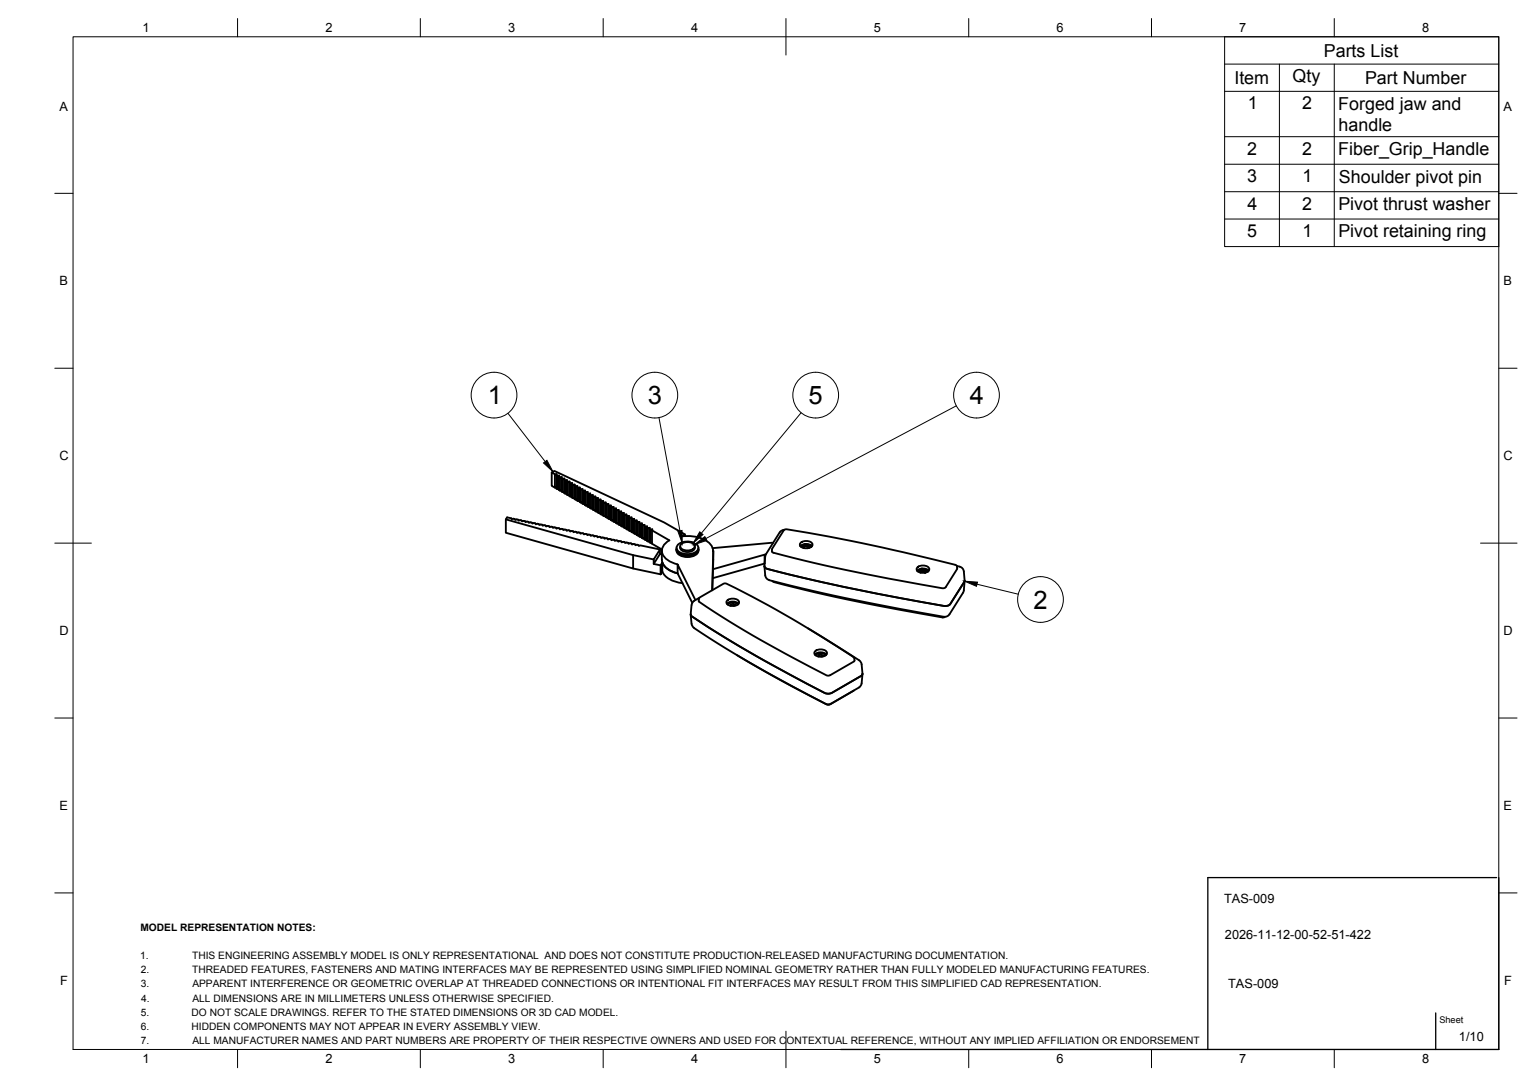
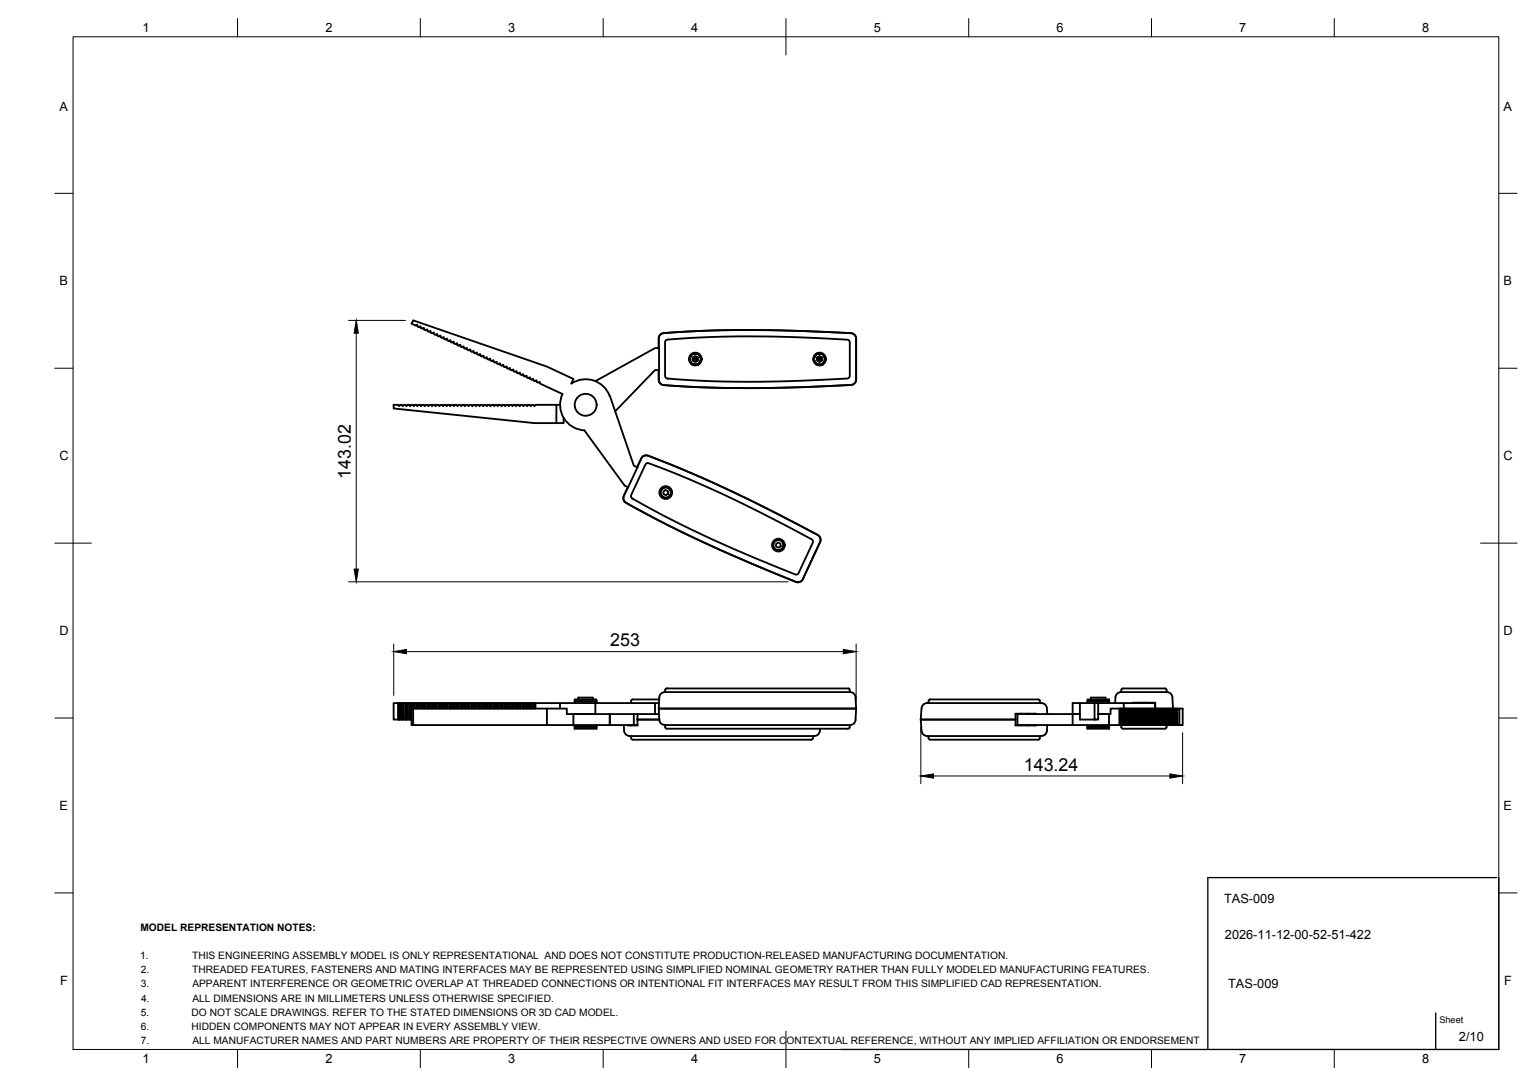
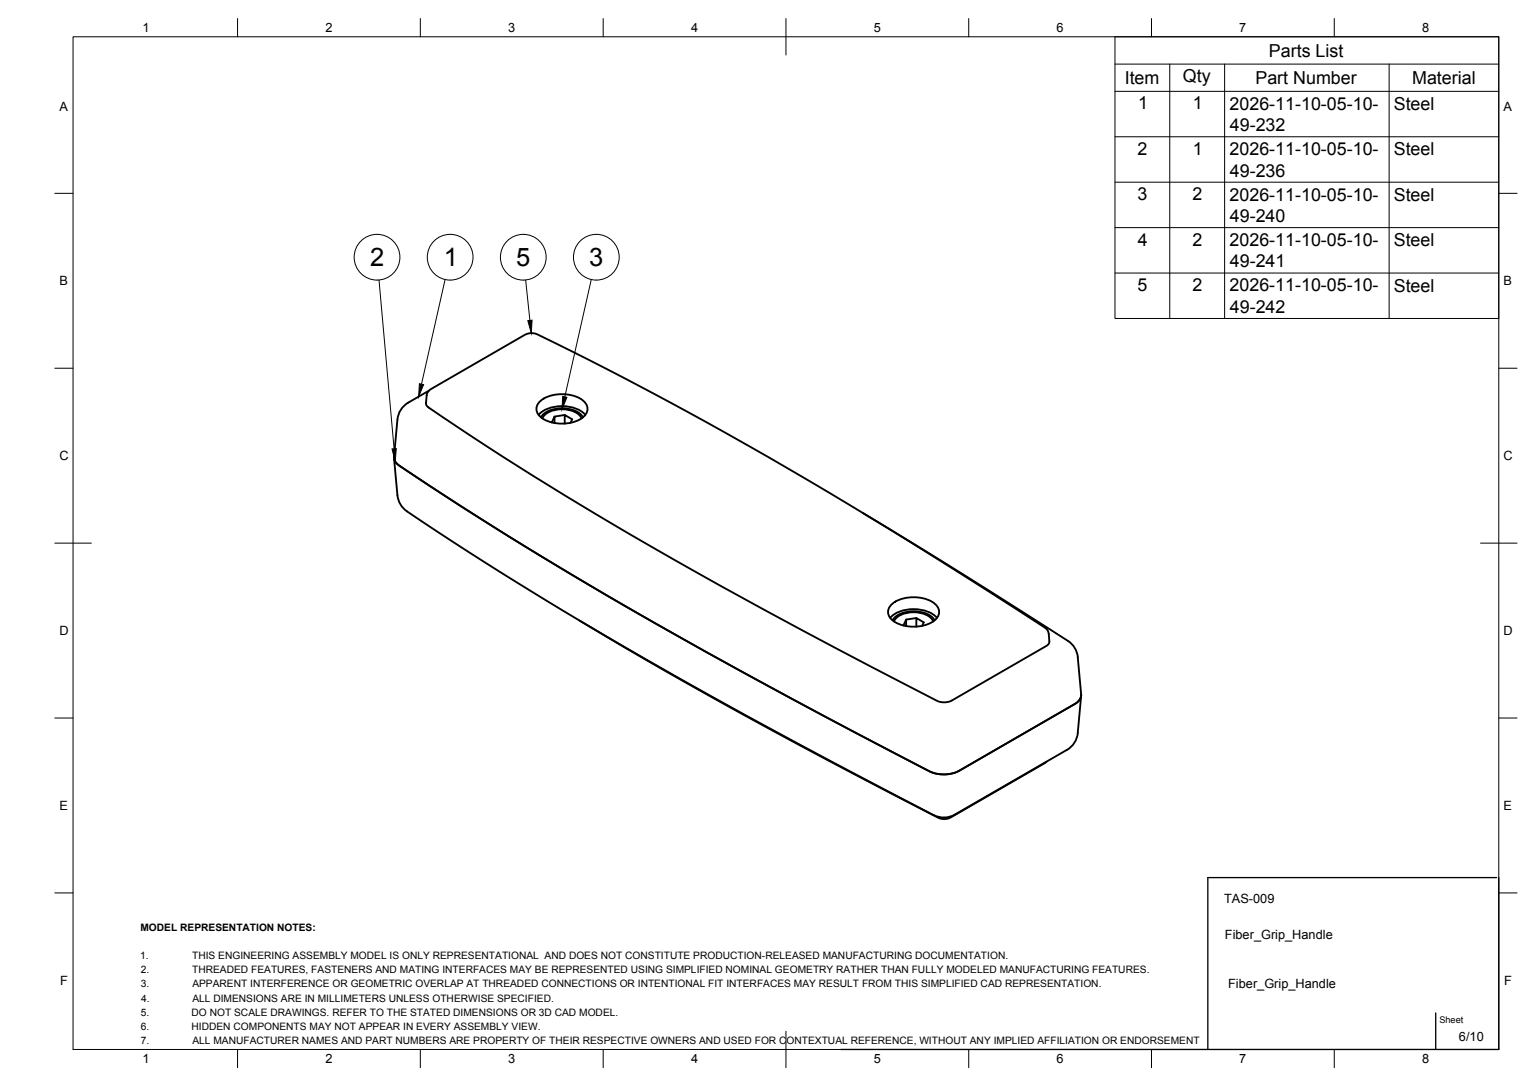
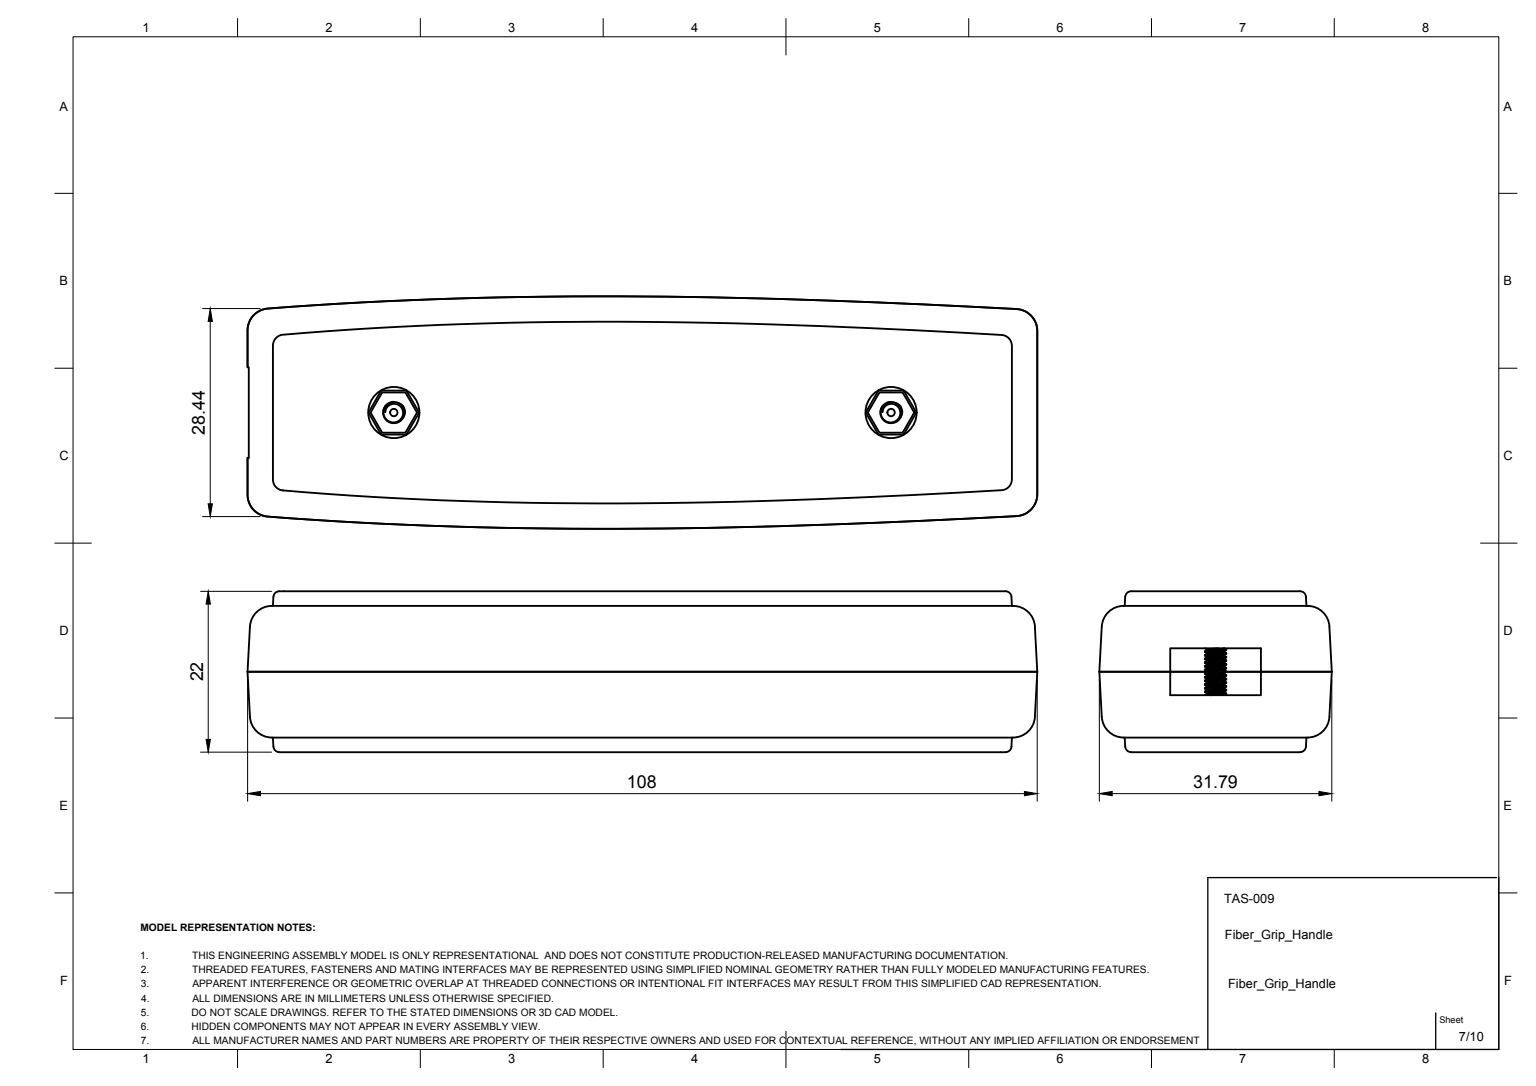
ISO-10303-21;
HEADER;
/* Generated by software containing ST-Developer
 * from STEP Tools, Inc. (www.steptools.com) 
 */

FILE_DESCRIPTION(
/* description */ (''),
/* implementation_level */ '2;1');

FILE_NAME(
/* name */ 'TAS-009.step',
/* time_stamp */ '2026-11-12T00:53:40-08:00',
/* author */ (''),
/* organization */ (''),
/* preprocessor_version */ 'ST-DEVELOPER v20.2',
/* originating_system */ 'Autodesk Translation Framework v15.17.0.0',
/* authorisation */ '');

FILE_SCHEMA (('AUTOMOTIVE_DESIGN { 1 0 10303 214 3 1 1 }'));
ENDSEC;

DATA;
#10=MECHANICAL_DESIGN_GEOMETRIC_PRESENTATION_REPRESENTATION('',(#572,#573,
#574,#575,#576,#577,#578,#579,#580),#22129);
#11=ITEM_DEFINED_TRANSFORMATION($,$,#9088,#9475);
#12=ITEM_DEFINED_TRANSFORMATION($,$,#9198,#9476);
#13=ITEM_DEFINED_TRANSFORMATION($,$,#9314,#9477);
#14=ITEM_DEFINED_TRANSFORMATION($,$,#9396,#9478);
#15=ITEM_DEFINED_TRANSFORMATION($,$,#9422,#9479);
#16=ITEM_DEFINED_TRANSFORMATION($,$,#9314,#9480);
#17=ITEM_DEFINED_TRANSFORMATION($,$,#9396,#9481);
#18=ITEM_DEFINED_TRANSFORMATION($,$,#9422,#9482);
#19=ITEM_DEFINED_TRANSFORMATION($,$,#8913,#9492);
#20=ITEM_DEFINED_TRANSFORMATION($,$,#9087,#9493);
#21=ITEM_DEFINED_TRANSFORMATION($,$,#8913,#9494);
#22=ITEM_DEFINED_TRANSFORMATION($,$,#9058,#9495);
#23=ITEM_DEFINED_TRANSFORMATION($,$,#9483,#9496);
#24=ITEM_DEFINED_TRANSFORMATION($,$,#9076,#9497);
#25=ITEM_DEFINED_TRANSFORMATION($,$,#9087,#9498);
#26=ITEM_DEFINED_TRANSFORMATION($,$,#9483,#9499);
#27=(
REPRESENTATION_RELATIONSHIP($,$,#22177,#22176)
REPRESENTATION_RELATIONSHIP_WITH_TRANSFORMATION(#11)
SHAPE_REPRESENTATION_RELATIONSHIP()
);
#28=(
REPRESENTATION_RELATIONSHIP($,$,#22178,#22176)
REPRESENTATION_RELATIONSHIP_WITH_TRANSFORMATION(#12)
SHAPE_REPRESENTATION_RELATIONSHIP()
);
#29=(
REPRESENTATION_RELATIONSHIP($,$,#22179,#22176)
REPRESENTATION_RELATIONSHIP_WITH_TRANSFORMATION(#13)
SHAPE_REPRESENTATION_RELATIONSHIP()
);
#30=(
REPRESENTATION_RELATIONSHIP($,$,#22180,#22176)
REPRESENTATION_RELATIONSHIP_WITH_TRANSFORMATION(#14)
SHAPE_REPRESENTATION_RELATIONSHIP()
);
#31=(
REPRESENTATION_RELATIONSHIP($,$,#22181,#22176)
REPRESENTATION_RELATIONSHIP_WITH_TRANSFORMATION(#15)
SHAPE_REPRESENTATION_RELATIONSHIP()
);
#32=(
REPRESENTATION_RELATIONSHIP($,$,#22179,#22176)
REPRESENTATION_RELATIONSHIP_WITH_TRANSFORMATION(#16)
SHAPE_REPRESENTATION_RELATIONSHIP()
);
#33=(
REPRESENTATION_RELATIONSHIP($,$,#22180,#22176)
REPRESENTATION_RELATIONSHIP_WITH_TRANSFORMATION(#17)
SHAPE_REPRESENTATION_RELATIONSHIP()
);
#34=(
REPRESENTATION_RELATIONSHIP($,$,#22181,#22176)
REPRESENTATION_RELATIONSHIP_WITH_TRANSFORMATION(#18)
SHAPE_REPRESENTATION_RELATIONSHIP()
);
#35=(
REPRESENTATION_RELATIONSHIP($,$,#22173,#22172)
REPRESENTATION_RELATIONSHIP_WITH_TRANSFORMATION(#19)
SHAPE_REPRESENTATION_RELATIONSHIP()
);
#36=(
REPRESENTATION_RELATIONSHIP($,$,#22176,#22172)
REPRESENTATION_RELATIONSHIP_WITH_TRANSFORMATION(#20)
SHAPE_REPRESENTATION_RELATIONSHIP()
);
#37=(
REPRESENTATION_RELATIONSHIP($,$,#22173,#22172)
REPRESENTATION_RELATIONSHIP_WITH_TRANSFORMATION(#21)
SHAPE_REPRESENTATION_RELATIONSHIP()
);
#38=(
REPRESENTATION_RELATIONSHIP($,$,#22174,#22172)
REPRESENTATION_RELATIONSHIP_WITH_TRANSFORMATION(#22)
SHAPE_REPRESENTATION_RELATIONSHIP()
);
#39=(
REPRESENTATION_RELATIONSHIP($,$,#22182,#22172)
REPRESENTATION_RELATIONSHIP_WITH_TRANSFORMATION(#23)
SHAPE_REPRESENTATION_RELATIONSHIP()
);
#40=(
REPRESENTATION_RELATIONSHIP($,$,#22175,#22172)
REPRESENTATION_RELATIONSHIP_WITH_TRANSFORMATION(#24)
SHAPE_REPRESENTATION_RELATIONSHIP()
);
#41=(
REPRESENTATION_RELATIONSHIP($,$,#22176,#22172)
REPRESENTATION_RELATIONSHIP_WITH_TRANSFORMATION(#25)
SHAPE_REPRESENTATION_RELATIONSHIP()
);
#42=(
REPRESENTATION_RELATIONSHIP($,$,#22182,#22172)
REPRESENTATION_RELATIONSHIP_WITH_TRANSFORMATION(#26)
SHAPE_REPRESENTATION_RELATIONSHIP()
);
#43=CONTEXT_DEPENDENT_SHAPE_REPRESENTATION(#27,#22155);
#44=CONTEXT_DEPENDENT_SHAPE_REPRESENTATION(#28,#22156);
#45=CONTEXT_DEPENDENT_SHAPE_REPRESENTATION(#29,#22157);
#46=CONTEXT_DEPENDENT_SHAPE_REPRESENTATION(#30,#22158);
#47=CONTEXT_DEPENDENT_SHAPE_REPRESENTATION(#31,#22159);
#48=CONTEXT_DEPENDENT_SHAPE_REPRESENTATION(#32,#22160);
#49=CONTEXT_DEPENDENT_SHAPE_REPRESENTATION(#33,#22161);
#50=CONTEXT_DEPENDENT_SHAPE_REPRESENTATION(#34,#22162);
#51=CONTEXT_DEPENDENT_SHAPE_REPRESENTATION(#35,#22164);
#52=CONTEXT_DEPENDENT_SHAPE_REPRESENTATION(#36,#22165);
#53=CONTEXT_DEPENDENT_SHAPE_REPRESENTATION(#37,#22166);
#54=CONTEXT_DEPENDENT_SHAPE_REPRESENTATION(#38,#22167);
#55=CONTEXT_DEPENDENT_SHAPE_REPRESENTATION(#39,#22168);
#56=CONTEXT_DEPENDENT_SHAPE_REPRESENTATION(#40,#22169);
#57=CONTEXT_DEPENDENT_SHAPE_REPRESENTATION(#41,#22170);
#58=CONTEXT_DEPENDENT_SHAPE_REPRESENTATION(#42,#22171);
#59=NEXT_ASSEMBLY_USAGE_OCCURRENCE('Upper structural shell:1',
'Upper structural shell:1','Upper structural shell:1',#22188,#22189,
'Upper structural shell:1');
#60=NEXT_ASSEMBLY_USAGE_OCCURRENCE('Lower structural shell:1',
'Lower structural shell:1','Lower structural shell:1',#22188,#22190,
'Lower structural shell:1');
#61=NEXT_ASSEMBLY_USAGE_OCCURRENCE('Socket head cap screw M3x16:1',
'Socket head cap screw M3x16:1','Socket head cap screw M3x16:1',#22188,
#22191,'Socket head cap screw M3x16:1');
#62=NEXT_ASSEMBLY_USAGE_OCCURRENCE('Hex nut M3:1','Hex nut M3:1',
'Hex nut M3:1',#22188,#22192,'Hex nut M3:1');
#63=NEXT_ASSEMBLY_USAGE_OCCURRENCE('Soft grip layer:1',
'Soft grip layer:1','Soft grip layer:1',#22188,#22193,
'Soft grip layer:1');
#64=NEXT_ASSEMBLY_USAGE_OCCURRENCE('Socket head cap screw M3x16:2',
'Socket head cap screw M3x16:2','Socket head cap screw M3x16:2',#22188,
#22191,'Socket head cap screw M3x16:2');
#65=NEXT_ASSEMBLY_USAGE_OCCURRENCE('Hex nut M3:2','Hex nut M3:2',
'Hex nut M3:2',#22188,#22192,'Hex nut M3:2');
#66=NEXT_ASSEMBLY_USAGE_OCCURRENCE('Soft grip layer:2',
'Soft grip layer:2','Soft grip layer:2',#22188,#22193,
'Soft grip layer:2');
#67=NEXT_ASSEMBLY_USAGE_OCCURRENCE('Forged jaw and handle:1',
'Forged jaw and handle:1','Forged jaw and handle:1',#22184,#22185,
'Forged jaw and handle:1');
#68=NEXT_ASSEMBLY_USAGE_OCCURRENCE('Fiber_Grip_Handle:1',
'Fiber_Grip_Handle:1','Fiber_Grip_Handle:1',#22184,#22188,
'Fiber_Grip_Handle:1');
#69=NEXT_ASSEMBLY_USAGE_OCCURRENCE('Forged jaw and handle:2',
'Forged jaw and handle:2','Forged jaw and handle:2',#22184,#22185,
'Forged jaw and handle:2');
#70=NEXT_ASSEMBLY_USAGE_OCCURRENCE('Shoulder pivot pin:1',
'Shoulder pivot pin:1','Shoulder pivot pin:1',#22184,#22186,
'Shoulder pivot pin:1');
#71=NEXT_ASSEMBLY_USAGE_OCCURRENCE('Pivot thrust washer:1',
'Pivot thrust washer:1','Pivot thrust washer:1',#22184,#22194,
'Pivot thrust washer:1');
#72=NEXT_ASSEMBLY_USAGE_OCCURRENCE('Pivot retaining ring:1',
'Pivot retaining ring:1','Pivot retaining ring:1',#22184,#22187,
'Pivot retaining ring:1');
#73=NEXT_ASSEMBLY_USAGE_OCCURRENCE('Fiber_Grip_Handle:2',
'Fiber_Grip_Handle:2','Fiber_Grip_Handle:2',#22184,#22188,
'Fiber_Grip_Handle:2');
#74=NEXT_ASSEMBLY_USAGE_OCCURRENCE('Pivot thrust washer:2',
'Pivot thrust washer:2','Pivot thrust washer:2',#22184,#22194,
'Pivot thrust washer:2');
#75=CONICAL_SURFACE('',#9377,0.1,0.785398163397448);
#76=SPHERICAL_SURFACE('',#9161,0.1);
#77=SPHERICAL_SURFACE('',#9164,0.0999999999999998);
#78=SPHERICAL_SURFACE('',#9168,0.0999999999999993);
#79=SPHERICAL_SURFACE('',#9172,0.1);
#80=SPHERICAL_SURFACE('',#9177,0.3);
#81=SPHERICAL_SURFACE('',#9181,0.3);
#82=SPHERICAL_SURFACE('',#9185,0.299999999999999);
#83=SPHERICAL_SURFACE('',#9190,0.3);
#84=SPHERICAL_SURFACE('',#9277,0.1);
#85=SPHERICAL_SURFACE('',#9280,0.0999999999999998);
#86=SPHERICAL_SURFACE('',#9284,0.0999999999999993);
#87=SPHERICAL_SURFACE('',#9288,0.1);
#88=SPHERICAL_SURFACE('',#9293,0.3);
#89=SPHERICAL_SURFACE('',#9297,0.3);
#90=SPHERICAL_SURFACE('',#9301,0.299999999999999);
#91=SPHERICAL_SURFACE('',#9306,0.3);
#92=B_SPLINE_SURFACE_WITH_KNOTS('',3,3,((#12365,#12366,#12367,#12368),(#12369,
#12370,#12371,#12372),(#12373,#12374,#12375,#12376),(#12377,#12378,#12379,
#12380),(#12381,#12382,#12383,#12384)),.UNSPECIFIED.,.F.,.F.,.F.,(4,1,4),
(4,4),(0.,0.571428571428571,1.),(1.0454440030657,3.44967454744645),
 .UNSPECIFIED.);
#93=B_SPLINE_SURFACE_WITH_KNOTS('',3,3,((#12457,#12458,#12459,#12460),(#12461,
#12462,#12463,#12464),(#12465,#12466,#12467,#12468),(#12469,#12470,#12471,
#12472),(#12473,#12474,#12475,#12476)),.UNSPECIFIED.,.F.,.F.,.F.,(4,1,4),
(4,4),(0.,0.571428571428571,1.),(7.24519303641511,9.95046872158573),
 .UNSPECIFIED.);
#94=B_SPLINE_SURFACE_WITH_KNOTS('',3,3,((#13338,#13339,#13340,#13341),(#13342,
#13343,#13344,#13345),(#13346,#13347,#13348,#13349),(#13350,#13351,#13352,
#13353)),.UNSPECIFIED.,.F.,.F.,.F.,(4,4),(4,4),(0.0705535719740953,0.323522444336189),
(0.0117434863834119,0.684857763552191),.UNSPECIFIED.);
#95=B_SPLINE_SURFACE_WITH_KNOTS('',3,3,((#13358,#13359,#13360,#13361),(#13362,
#13363,#13364,#13365),(#13366,#13367,#13368,#13369),(#13370,#13371,#13372,
#13373)),.UNSPECIFIED.,.F.,.F.,.F.,(4,4),(4,4),(0.0262419052680539,0.0545428296147404),
(0.0121538053864343,0.684980602226481),.UNSPECIFIED.);
#96=B_SPLINE_SURFACE_WITH_KNOTS('',3,3,((#13383,#13384,#13385,#13386),(#13387,
#13388,#13389,#13390),(#13391,#13392,#13393,#13394),(#13395,#13396,#13397,
#13398),(#13399,#13400,#13401,#13402)),.UNSPECIFIED.,.F.,.F.,.F.,(4,1,4),
(4,4),(0.,0.571428571428571,1.),(0.752061768057538,3.45733745322815),
 .UNSPECIFIED.);
#97=B_SPLINE_SURFACE_WITH_KNOTS('',3,3,((#13403,#13404,#13405,#13406),(#13407,
#13408,#13409,#13410),(#13411,#13412,#13413,#13414),(#13415,#13416,#13417,
#13418),(#13419,#13420,#13421,#13422)),.UNSPECIFIED.,.F.,.F.,.F.,(4,1,4),
(4,4),(0.,0.571428571428571,1.),(0.283259008618247,0.557056952888827),
 .UNSPECIFIED.);
#98=B_SPLINE_SURFACE_WITH_KNOTS('',3,3,((#13436,#13437,#13438,#13439),(#13440,
#13441,#13442,#13443),(#13444,#13445,#13446,#13447),(#13448,#13449,#13450,
#13451)),.UNSPECIFIED.,.F.,.F.,.F.,(4,4),(4,4),(0.67647755566375,0.929446428026011),
(0.0117434863436937,0.684857763580381),.UNSPECIFIED.);
#99=B_SPLINE_SURFACE_WITH_KNOTS('',3,3,((#13452,#13453,#13454,#13455),(#13456,
#13457,#13458,#13459),(#13460,#13461,#13462,#13463),(#13464,#13465,#13466,
#13467)),.UNSPECIFIED.,.F.,.F.,.F.,(4,4),(4,4),(0.945457170385156,0.973758094731946),
(0.0121538053598088,0.684980602226481),.UNSPECIFIED.);
#100=B_SPLINE_SURFACE_WITH_KNOTS('',3,3,((#13551,#13552,#13553,#13554),
(#13555,#13556,#13557,#13558),(#13559,#13560,#13561,#13562),(#13563,#13564,
#13565,#13566)),.UNSPECIFIED.,.F.,.F.,.F.,(4,4),(4,4),(0.341142793678372,
0.658675488550287),(0.0116221239297273,0.684255166525269),.UNSPECIFIED.);
#101=B_SPLINE_SURFACE_WITH_KNOTS('',3,3,((#13571,#13572,#13573,#13574),
(#13575,#13576,#13577,#13578),(#13579,#13580,#13581,#13582),(#13583,#13584,
#13585,#13586),(#13587,#13588,#13589,#13590)),.UNSPECIFIED.,.F.,.F.,.F.,
(4,1,4),(4,4),(0.,0.571428571428571,1.),(3.65450559744172,7.0548588409572),
 .UNSPECIFIED.);
#102=B_SPLINE_SURFACE_WITH_KNOTS('',3,3,((#13600,#13601,#13602,#13603),
(#13604,#13605,#13606,#13607),(#13608,#13609,#13610,#13611),(#13612,#13613,
#13614,#13615),(#13616,#13617,#13618,#13619)),.UNSPECIFIED.,.F.,.F.,.F.,
(4,1,4),(4,4),(0.,0.571428571428571,1.),(3.64767164868607,7.04802489220155),
 .UNSPECIFIED.);
#103=B_SPLINE_SURFACE_WITH_KNOTS('',3,3,((#13624,#13625,#13626,#13627),
(#13628,#13629,#13630,#13631),(#13632,#13633,#13634,#13635),(#13636,#13637,
#13638,#13639)),.UNSPECIFIED.,.F.,.F.,.F.,(4,4),(4,4),(0.341324511449716,
0.658857206321627),(0.0116221214776208,0.684255166525269),.UNSPECIFIED.);
#104=B_SPLINE_SURFACE_WITH_KNOTS('',3,3,((#13684,#13685,#13686,#13687),
(#13688,#13689,#13690,#13691),(#13692,#13693,#13694,#13695),(#13696,#13697,
#13698,#13699)),.UNSPECIFIED.,.F.,.F.,.F.,(4,4),(4,4),(0.676316266718331,
0.901708040522105),(0.0117102006467275,0.68495201331719),.UNSPECIFIED.);
#105=B_SPLINE_SURFACE_WITH_KNOTS('',3,3,((#13704,#13705,#13706,#13707),
(#13708,#13709,#13710,#13711),(#13712,#13713,#13714,#13715),(#13716,#13717,
#13718,#13719),(#13720,#13721,#13722,#13723)),.UNSPECIFIED.,.F.,.F.,.F.,
(4,1,4),(4,4),(0.,0.571428571428571,1.),(7.25285594219682,9.65708648657758),
 .UNSPECIFIED.);
#106=B_SPLINE_SURFACE_WITH_KNOTS('',3,3,((#13733,#13734,#13735,#13736),
(#13737,#13738,#13739,#13740),(#13741,#13742,#13743,#13744),(#13745,#13746,
#13747,#13748)),.UNSPECIFIED.,.F.,.F.,.F.,(4,4),(4,4),(0.0982919594778951,
0.323683733281714),(0.0117102006467272,0.68495201331719),.UNSPECIFIED.);
#107=B_SPLINE_SURFACE_WITH_KNOTS('',3,3,((#13823,#13824,#13825,#13826),
(#13827,#13828,#13829,#13830),(#13831,#13832,#13833,#13834),(#13835,#13836,
#13837,#13838)),.UNSPECIFIED.,.F.,.F.,.F.,(4,4),(4,4),(0.917922863855343,
0.974411608827007),(0.0122403473423911,0.685344304754238),.UNSPECIFIED.);
#108=B_SPLINE_SURFACE_WITH_KNOTS('',3,3,((#13848,#13849,#13850,#13851),
(#13852,#13853,#13854,#13855),(#13856,#13857,#13858,#13859),(#13860,#13861,
#13862,#13863),(#13864,#13865,#13866,#13867)),.UNSPECIFIED.,.F.,.F.,.F.,
(4,1,4),(4,4),(0.,0.571428571428571,1.),(9.85085636625011,10.4271318523291),
 .UNSPECIFIED.);
#109=B_SPLINE_SURFACE_WITH_KNOTS('',3,3,((#13881,#13882,#13883,#13884),
(#13885,#13886,#13887,#13888),(#13889,#13890,#13891,#13892),(#13893,#13894,
#13895,#13896)),.UNSPECIFIED.,.F.,.F.,.F.,(4,4),(4,4),(0.025588391172993,
0.0820771361446569),(0.0122403473423911,0.685344304754238),
 .UNSPECIFIED.);
#110=B_SPLINE_SURFACE_WITH_KNOTS('',3,3,((#13906,#13907,#13908,#13909),
(#13910,#13911,#13912,#13913),(#13914,#13915,#13916,#13917),(#13918,#13919,
#13920,#13921),(#13922,#13923,#13924,#13925)),.UNSPECIFIED.,.F.,.F.,.F.,
(4,1,4),(4,4),(0.,0.571428571428571,1.),(0.27539863731415,0.851674123393175),
 .UNSPECIFIED.);
#111=B_SPLINE_SURFACE_WITH_KNOTS('',3,3,((#13939,#13940,#13941,#13942),
(#13943,#13944,#13945,#13946),(#13947,#13948,#13949,#13950),(#13951,#13952,
#13953,#13954),(#13955,#13956,#13957,#13958)),.UNSPECIFIED.,.F.,.F.,.F.,
(4,1,4),(4,4),(0.,0.571428571428571,1.),(0.00944995813270487,0.618489359031386),
 .UNSPECIFIED.);
#112=B_SPLINE_SURFACE_WITH_KNOTS('',3,3,((#13965,#13966,#13967,#13968),
(#13969,#13970,#13971,#13972),(#13973,#13974,#13975,#13976),(#13977,#13978,
#13979,#13980),(#13981,#13982,#13983,#13984)),.UNSPECIFIED.,.F.,.F.,.F.,
(4,1,4),(4,4),(0.,0.571428571428571,1.),(0.00908570715245136,0.618164468641375),
 .UNSPECIFIED.);
#113=B_SPLINE_SURFACE_WITH_KNOTS('',3,3,((#13989,#13990,#13991,#13992),
(#13993,#13994,#13995,#13996),(#13997,#13998,#13999,#14000),(#14001,#14002,
#14003,#14004),(#14005,#14006,#14007,#14008)),.UNSPECIFIED.,.F.,.F.,.F.,
(4,1,4),(4,4),(0.,0.571428571428571,1.),(0.0091183540525243,0.618164468641375),
 .UNSPECIFIED.);
#114=B_SPLINE_SURFACE_WITH_KNOTS('',3,3,((#14013,#14014,#14015,#14016),
(#14017,#14018,#14019,#14020),(#14021,#14022,#14023,#14024),(#14025,#14026,
#14027,#14028),(#14029,#14030,#14031,#14032)),.UNSPECIFIED.,.F.,.F.,.F.,
(4,1,4),(4,4),(0.,0.571428571428571,1.),(10.1454735367545,10.419271481025),
 .UNSPECIFIED.);
#115=B_SPLINE_SURFACE_WITH_KNOTS('',3,3,((#14033,#14034,#14035,#14036),
(#14037,#14038,#14039,#14040),(#14041,#14042,#14043,#14044),(#14045,#14046,
#14047,#14048),(#14049,#14050,#14051,#14052)),.UNSPECIFIED.,.F.,.F.,.F.,
(4,1,4),(4,4),(0.,0.571428571428571,1.),(0.0094045468285345,0.618489359031386),
 .UNSPECIFIED.);
#116=B_SPLINE_SURFACE_WITH_KNOTS('',3,3,((#14078,#14079,#14080,#14081),
(#14082,#14083,#14084,#14085),(#14086,#14087,#14088,#14089),(#14090,#14091,
#14092,#14093),(#14094,#14095,#14096,#14097)),.UNSPECIFIED.,.F.,.F.,.F.,
(4,1,4),(4,4),(0.,0.571428571428571,1.),(-0.00535061636073277,0.618489359031386),
 .UNSPECIFIED.);
#117=B_SPLINE_SURFACE_WITH_KNOTS('',3,3,((#14116,#14117,#14118,#14119,#14120),
(#14121,#14122,#14123,#14124,#14125),(#14126,#14127,#14128,#14129,#14130),
(#14131,#14132,#14133,#14134,#14135),(#14136,#14137,#14138,#14139,#14140)),
 .UNSPECIFIED.,.F.,.F.,.F.,(4,1,4),(4,1,4),(0.,0.571428571428571,1.),(0.283259008618247,
4.63063308449434,10.4271318523291),.UNSPECIFIED.);
#118=B_SPLINE_SURFACE_WITH_KNOTS('',3,3,((#14151,#14152,#14153,#14154),
(#14155,#14156,#14157,#14158),(#14159,#14160,#14161,#14162),(#14163,#14164,
#14165,#14166),(#14167,#14168,#14169,#14170)),.UNSPECIFIED.,.F.,.F.,.F.,
(4,1,4),(4,4),(0.,0.571428571428571,1.),(-0.00578978989683084,0.618164468641375),
 .UNSPECIFIED.);
#119=B_SPLINE_SURFACE_WITH_KNOTS('',3,3,((#14179,#14180,#14181,#14182),
(#14183,#14184,#14185,#14186),(#14187,#14188,#14189,#14190),(#14191,#14192,
#14193,#14194),(#14195,#14196,#14197,#14198)),.UNSPECIFIED.,.F.,.F.,.F.,
(4,1,4),(4,4),(0.,0.571428571428571,1.),(-0.00569189159989896,0.618164468641375),
 .UNSPECIFIED.);
#120=B_SPLINE_SURFACE_WITH_KNOTS('',3,3,((#14207,#14208,#14209,#14210,#14211),
(#14212,#14213,#14214,#14215,#14216),(#14217,#14218,#14219,#14220,#14221),
(#14222,#14223,#14224,#14225,#14226),(#14227,#14228,#14229,#14230,#14231)),
 .UNSPECIFIED.,.F.,.F.,.F.,(4,1,4),(4,1,4),(0.,0.571428571428571,1.),(0.27539863731415,
4.62277271319024,10.419271481025),.UNSPECIFIED.);
#121=B_SPLINE_SURFACE_WITH_KNOTS('',3,3,((#14242,#14243,#14244,#14245),
(#14246,#14247,#14248,#14249),(#14250,#14251,#14252,#14253),(#14254,#14255,
#14256,#14257),(#14258,#14259,#14260,#14261)),.UNSPECIFIED.,.F.,.F.,.F.,
(4,1,4),(4,4),(0.,0.571428571428571,1.),(-0.0054868135546625,0.618489359031386),
 .UNSPECIFIED.);
#122=B_SPLINE_SURFACE_WITH_KNOTS('',3,3,((#14270,#14271,#14272,#14273),
(#14274,#14275,#14276,#14277),(#14278,#14279,#14280,#14281),(#14282,#14283,
#14284,#14285)),.UNSPECIFIED.,.F.,.F.,.F.,(4,4),(4,4),(0.026239262514127,
0.974414173651419),(0.,0.685344304754238),.UNSPECIFIED.);
#123=B_SPLINE_SURFACE_WITH_KNOTS('',3,3,((#14288,#14289,#14290,#14291),
(#14292,#14293,#14294,#14295),(#14296,#14297,#14298,#14299),(#14300,#14301,
#14302,#14303)),.UNSPECIFIED.,.F.,.F.,.F.,(4,4),(4,4),(0.0255858263485814,
0.973760737485873),(0.,0.685344304754238),.UNSPECIFIED.);
#124=B_SPLINE_SURFACE_WITH_KNOTS('',3,3,((#14410,#14411,#14412,#14413),
(#14414,#14415,#14416,#14417),(#14418,#14419,#14420,#14421),(#14422,#14423,
#14424,#14425),(#14426,#14427,#14428,#14429)),.UNSPECIFIED.,.F.,.F.,.F.,
(4,1,4),(4,4),(0.,0.571428571428571,1.),(1.0454440030657,3.44967454744645),
 .UNSPECIFIED.);
#125=B_SPLINE_SURFACE_WITH_KNOTS('',3,3,((#14502,#14503,#14504,#14505),
(#14506,#14507,#14508,#14509),(#14510,#14511,#14512,#14513),(#14514,#14515,
#14516,#14517),(#14518,#14519,#14520,#14521)),.UNSPECIFIED.,.F.,.F.,.F.,
(4,1,4),(4,4),(0.,0.571428571428571,1.),(7.24519303641511,9.95046872158573),
 .UNSPECIFIED.);
#126=B_SPLINE_SURFACE_WITH_KNOTS('',3,3,((#15443,#15444,#15445,#15446),
(#15447,#15448,#15449,#15450),(#15451,#15452,#15453,#15454),(#15455,#15456,
#15457,#15458)),.UNSPECIFIED.,.F.,.F.,.F.,(4,4),(4,4),(0.0705535719740953,
0.323522444336189),(0.0117434863834119,0.684857763552191),.UNSPECIFIED.);
#127=B_SPLINE_SURFACE_WITH_KNOTS('',3,3,((#15463,#15464,#15465,#15466),
(#15467,#15468,#15469,#15470),(#15471,#15472,#15473,#15474),(#15475,#15476,
#15477,#15478)),.UNSPECIFIED.,.F.,.F.,.F.,(4,4),(4,4),(0.0262419052680539,
0.0545428296147404),(0.0121538053864343,0.684980602226481),
 .UNSPECIFIED.);
#128=B_SPLINE_SURFACE_WITH_KNOTS('',3,3,((#15488,#15489,#15490,#15491),
(#15492,#15493,#15494,#15495),(#15496,#15497,#15498,#15499),(#15500,#15501,
#15502,#15503),(#15504,#15505,#15506,#15507)),.UNSPECIFIED.,.F.,.F.,.F.,
(4,1,4),(4,4),(0.,0.571428571428571,1.),(0.752061768057538,3.45733745322815),
 .UNSPECIFIED.);
#129=B_SPLINE_SURFACE_WITH_KNOTS('',3,3,((#15508,#15509,#15510,#15511),
(#15512,#15513,#15514,#15515),(#15516,#15517,#15518,#15519),(#15520,#15521,
#15522,#15523),(#15524,#15525,#15526,#15527)),.UNSPECIFIED.,.F.,.F.,.F.,
(4,1,4),(4,4),(0.,0.571428571428571,1.),(0.283259008618247,0.557056952888827),
 .UNSPECIFIED.);
#130=B_SPLINE_SURFACE_WITH_KNOTS('',3,3,((#15541,#15542,#15543,#15544),
(#15545,#15546,#15547,#15548),(#15549,#15550,#15551,#15552),(#15553,#15554,
#15555,#15556)),.UNSPECIFIED.,.F.,.F.,.F.,(4,4),(4,4),(0.67647755566375,
0.929446428026011),(0.0117434863436937,0.684857763580381),.UNSPECIFIED.);
#131=B_SPLINE_SURFACE_WITH_KNOTS('',3,3,((#15557,#15558,#15559,#15560),
(#15561,#15562,#15563,#15564),(#15565,#15566,#15567,#15568),(#15569,#15570,
#15571,#15572)),.UNSPECIFIED.,.F.,.F.,.F.,(4,4),(4,4),(0.945457170385156,
0.973758094731946),(0.0121538053598088,0.684980602226481),.UNSPECIFIED.);
#132=B_SPLINE_SURFACE_WITH_KNOTS('',3,3,((#15656,#15657,#15658,#15659),
(#15660,#15661,#15662,#15663),(#15664,#15665,#15666,#15667),(#15668,#15669,
#15670,#15671)),.UNSPECIFIED.,.F.,.F.,.F.,(4,4),(4,4),(0.341142793678372,
0.658675488550287),(0.0116221239297273,0.684255166525269),.UNSPECIFIED.);
#133=B_SPLINE_SURFACE_WITH_KNOTS('',3,3,((#15676,#15677,#15678,#15679),
(#15680,#15681,#15682,#15683),(#15684,#15685,#15686,#15687),(#15688,#15689,
#15690,#15691),(#15692,#15693,#15694,#15695)),.UNSPECIFIED.,.F.,.F.,.F.,
(4,1,4),(4,4),(0.,0.571428571428571,1.),(3.65450559744172,7.0548588409572),
 .UNSPECIFIED.);
#134=B_SPLINE_SURFACE_WITH_KNOTS('',3,3,((#15705,#15706,#15707,#15708),
(#15709,#15710,#15711,#15712),(#15713,#15714,#15715,#15716),(#15717,#15718,
#15719,#15720),(#15721,#15722,#15723,#15724)),.UNSPECIFIED.,.F.,.F.,.F.,
(4,1,4),(4,4),(0.,0.571428571428571,1.),(3.64767164868607,7.04802489220155),
 .UNSPECIFIED.);
#135=B_SPLINE_SURFACE_WITH_KNOTS('',3,3,((#15729,#15730,#15731,#15732),
(#15733,#15734,#15735,#15736),(#15737,#15738,#15739,#15740),(#15741,#15742,
#15743,#15744)),.UNSPECIFIED.,.F.,.F.,.F.,(4,4),(4,4),(0.341324511449716,
0.658857206321627),(0.0116221214776208,0.684255166525269),.UNSPECIFIED.);
#136=B_SPLINE_SURFACE_WITH_KNOTS('',3,3,((#15789,#15790,#15791,#15792),
(#15793,#15794,#15795,#15796),(#15797,#15798,#15799,#15800),(#15801,#15802,
#15803,#15804)),.UNSPECIFIED.,.F.,.F.,.F.,(4,4),(4,4),(0.676316266718331,
0.901708040522105),(0.0117102006467275,0.68495201331719),.UNSPECIFIED.);
#137=B_SPLINE_SURFACE_WITH_KNOTS('',3,3,((#15809,#15810,#15811,#15812),
(#15813,#15814,#15815,#15816),(#15817,#15818,#15819,#15820),(#15821,#15822,
#15823,#15824),(#15825,#15826,#15827,#15828)),.UNSPECIFIED.,.F.,.F.,.F.,
(4,1,4),(4,4),(0.,0.571428571428571,1.),(7.25285594219682,9.65708648657758),
 .UNSPECIFIED.);
#138=B_SPLINE_SURFACE_WITH_KNOTS('',3,3,((#15838,#15839,#15840,#15841),
(#15842,#15843,#15844,#15845),(#15846,#15847,#15848,#15849),(#15850,#15851,
#15852,#15853)),.UNSPECIFIED.,.F.,.F.,.F.,(4,4),(4,4),(0.0982919594778951,
0.323683733281714),(0.0117102006467272,0.68495201331719),.UNSPECIFIED.);
#139=B_SPLINE_SURFACE_WITH_KNOTS('',3,3,((#15928,#15929,#15930,#15931),
(#15932,#15933,#15934,#15935),(#15936,#15937,#15938,#15939),(#15940,#15941,
#15942,#15943)),.UNSPECIFIED.,.F.,.F.,.F.,(4,4),(4,4),(0.917922863855343,
0.974411608827007),(0.0122403473423911,0.685344304754238),.UNSPECIFIED.);
#140=B_SPLINE_SURFACE_WITH_KNOTS('',3,3,((#15953,#15954,#15955,#15956),
(#15957,#15958,#15959,#15960),(#15961,#15962,#15963,#15964),(#15965,#15966,
#15967,#15968),(#15969,#15970,#15971,#15972)),.UNSPECIFIED.,.F.,.F.,.F.,
(4,1,4),(4,4),(0.,0.571428571428571,1.),(9.85085636625011,10.4271318523291),
 .UNSPECIFIED.);
#141=B_SPLINE_SURFACE_WITH_KNOTS('',3,3,((#15986,#15987,#15988,#15989),
(#15990,#15991,#15992,#15993),(#15994,#15995,#15996,#15997),(#15998,#15999,
#16000,#16001)),.UNSPECIFIED.,.F.,.F.,.F.,(4,4),(4,4),(0.025588391172993,
0.0820771361446569),(0.0122403473423911,0.685344304754238),
 .UNSPECIFIED.);
#142=B_SPLINE_SURFACE_WITH_KNOTS('',3,3,((#16011,#16012,#16013,#16014),
(#16015,#16016,#16017,#16018),(#16019,#16020,#16021,#16022),(#16023,#16024,
#16025,#16026),(#16027,#16028,#16029,#16030)),.UNSPECIFIED.,.F.,.F.,.F.,
(4,1,4),(4,4),(0.,0.571428571428571,1.),(0.27539863731415,0.851674123393175),
 .UNSPECIFIED.);
#143=B_SPLINE_SURFACE_WITH_KNOTS('',3,3,((#16044,#16045,#16046,#16047),
(#16048,#16049,#16050,#16051),(#16052,#16053,#16054,#16055),(#16056,#16057,
#16058,#16059),(#16060,#16061,#16062,#16063)),.UNSPECIFIED.,.F.,.F.,.F.,
(4,1,4),(4,4),(0.,0.571428571428571,1.),(0.00944995813270487,0.618489359031386),
 .UNSPECIFIED.);
#144=B_SPLINE_SURFACE_WITH_KNOTS('',3,3,((#16070,#16071,#16072,#16073),
(#16074,#16075,#16076,#16077),(#16078,#16079,#16080,#16081),(#16082,#16083,
#16084,#16085),(#16086,#16087,#16088,#16089)),.UNSPECIFIED.,.F.,.F.,.F.,
(4,1,4),(4,4),(0.,0.571428571428571,1.),(0.00908570715245136,0.618164468641375),
 .UNSPECIFIED.);
#145=B_SPLINE_SURFACE_WITH_KNOTS('',3,3,((#16094,#16095,#16096,#16097),
(#16098,#16099,#16100,#16101),(#16102,#16103,#16104,#16105),(#16106,#16107,
#16108,#16109),(#16110,#16111,#16112,#16113)),.UNSPECIFIED.,.F.,.F.,.F.,
(4,1,4),(4,4),(0.,0.571428571428571,1.),(0.0091183540525243,0.618164468641375),
 .UNSPECIFIED.);
#146=B_SPLINE_SURFACE_WITH_KNOTS('',3,3,((#16118,#16119,#16120,#16121),
(#16122,#16123,#16124,#16125),(#16126,#16127,#16128,#16129),(#16130,#16131,
#16132,#16133),(#16134,#16135,#16136,#16137)),.UNSPECIFIED.,.F.,.F.,.F.,
(4,1,4),(4,4),(0.,0.571428571428571,1.),(10.1454735367545,10.419271481025),
 .UNSPECIFIED.);
#147=B_SPLINE_SURFACE_WITH_KNOTS('',3,3,((#16138,#16139,#16140,#16141),
(#16142,#16143,#16144,#16145),(#16146,#16147,#16148,#16149),(#16150,#16151,
#16152,#16153),(#16154,#16155,#16156,#16157)),.UNSPECIFIED.,.F.,.F.,.F.,
(4,1,4),(4,4),(0.,0.571428571428571,1.),(0.0094045468285345,0.618489359031386),
 .UNSPECIFIED.);
#148=B_SPLINE_SURFACE_WITH_KNOTS('',3,3,((#16183,#16184,#16185,#16186),
(#16187,#16188,#16189,#16190),(#16191,#16192,#16193,#16194),(#16195,#16196,
#16197,#16198),(#16199,#16200,#16201,#16202)),.UNSPECIFIED.,.F.,.F.,.F.,
(4,1,4),(4,4),(0.,0.571428571428571,1.),(-0.00535061636073277,0.618489359031386),
 .UNSPECIFIED.);
#149=B_SPLINE_SURFACE_WITH_KNOTS('',3,3,((#16221,#16222,#16223,#16224,#16225),
(#16226,#16227,#16228,#16229,#16230),(#16231,#16232,#16233,#16234,#16235),
(#16236,#16237,#16238,#16239,#16240),(#16241,#16242,#16243,#16244,#16245)),
 .UNSPECIFIED.,.F.,.F.,.F.,(4,1,4),(4,1,4),(0.,0.571428571428571,1.),(0.283259008618247,
4.63063308449434,10.4271318523291),.UNSPECIFIED.);
#150=B_SPLINE_SURFACE_WITH_KNOTS('',3,3,((#16256,#16257,#16258,#16259),
(#16260,#16261,#16262,#16263),(#16264,#16265,#16266,#16267),(#16268,#16269,
#16270,#16271),(#16272,#16273,#16274,#16275)),.UNSPECIFIED.,.F.,.F.,.F.,
(4,1,4),(4,4),(0.,0.571428571428571,1.),(-0.00578978989683084,0.618164468641375),
 .UNSPECIFIED.);
#151=B_SPLINE_SURFACE_WITH_KNOTS('',3,3,((#16284,#16285,#16286,#16287),
(#16288,#16289,#16290,#16291),(#16292,#16293,#16294,#16295),(#16296,#16297,
#16298,#16299),(#16300,#16301,#16302,#16303)),.UNSPECIFIED.,.F.,.F.,.F.,
(4,1,4),(4,4),(0.,0.571428571428571,1.),(-0.00569189159989896,0.618164468641375),
 .UNSPECIFIED.);
#152=B_SPLINE_SURFACE_WITH_KNOTS('',3,3,((#16312,#16313,#16314,#16315,#16316),
(#16317,#16318,#16319,#16320,#16321),(#16322,#16323,#16324,#16325,#16326),
(#16327,#16328,#16329,#16330,#16331),(#16332,#16333,#16334,#16335,#16336)),
 .UNSPECIFIED.,.F.,.F.,.F.,(4,1,4),(4,1,4),(0.,0.571428571428571,1.),(0.27539863731415,
4.62277271319024,10.419271481025),.UNSPECIFIED.);
#153=B_SPLINE_SURFACE_WITH_KNOTS('',3,3,((#16347,#16348,#16349,#16350),
(#16351,#16352,#16353,#16354),(#16355,#16356,#16357,#16358),(#16359,#16360,
#16361,#16362),(#16363,#16364,#16365,#16366)),.UNSPECIFIED.,.F.,.F.,.F.,
(4,1,4),(4,4),(0.,0.571428571428571,1.),(-0.0054868135546625,0.618489359031386),
 .UNSPECIFIED.);
#154=B_SPLINE_SURFACE_WITH_KNOTS('',3,3,((#16375,#16376,#16377,#16378),
(#16379,#16380,#16381,#16382),(#16383,#16384,#16385,#16386),(#16387,#16388,
#16389,#16390)),.UNSPECIFIED.,.F.,.F.,.F.,(4,4),(4,4),(0.026239262514127,
0.974414173651419),(0.,0.685344304754238),.UNSPECIFIED.);
#155=B_SPLINE_SURFACE_WITH_KNOTS('',3,3,((#16393,#16394,#16395,#16396),
(#16397,#16398,#16399,#16400),(#16401,#16402,#16403,#16404),(#16405,#16406,
#16407,#16408)),.UNSPECIFIED.,.F.,.F.,.F.,(4,4),(4,4),(0.0255858263485814,
0.973760737485873),(0.,0.685344304754238),.UNSPECIFIED.);
#156=B_SPLINE_SURFACE_WITH_KNOTS('',3,3,((#18792,#18793,#18794,#18795,#18796,
#18797,#18798,#18799,#18800,#18801,#18802,#18803,#18804,#18805,#18806,#18807,
#18808,#18809,#18810,#18811,#18812,#18813,#18814,#18815,#18816,#18817,#18818,
#18819,#18820,#18821,#18822,#18823,#18824,#18825,#18826,#18827,#18828,#18829,
#18830,#18831,#18832,#18833,#18834,#18835,#18836,#18837,#18838,#18839,#18840,
#18841,#18842,#18843,#18844,#18845,#18846,#18847,#18848,#18849,#18850,#18851,
#18852,#18853,#18854,#18855,#18856,#18857,#18858,#18859,#18860,#18861,#18862,
#18863,#18864,#18865,#18866,#18867,#18868,#18869,#18870,#18871,#18872,#18873,
#18874,#18875,#18876,#18877,#18878,#18879,#18880,#18881,#18882,#18883,#18884,
#18885,#18886,#18887,#18888,#18889,#18890,#18891,#18892,#18893,#18894,#18895,
#18896,#18897,#18898,#18899,#18900,#18901,#18902,#18903,#18904,#18905,#18906,
#18907,#18908,#18909,#18910,#18911,#18912,#18913,#18914,#18915,#18916,#18917,
#18918,#18919,#18920,#18921,#18922,#18923,#18924,#18925,#18926,#18927,#18928,
#18929,#18930,#18931,#18932,#18933,#18934,#18935,#18936,#18937,#18938,#18939,
#18940,#18941,#18942,#18943,#18944,#18945,#18946,#18947,#18948,#18949,#18950,
#18951,#18952,#18953,#18954,#18955,#18956,#18957,#18958,#18959,#18960,#18961,
#18962,#18963,#18964,#18965,#18966,#18967,#18968,#18969,#18970,#18971,#18972,
#18973,#18974,#18975,#18976,#18977,#18978,#18979,#18980,#18981,#18982,#18983,
#18984,#18985,#18986,#18987),(#18988,#18989,#18990,#18991,#18992,#18993,
#18994,#18995,#18996,#18997,#18998,#18999,#19000,#19001,#19002,#19003,#19004,
#19005,#19006,#19007,#19008,#19009,#19010,#19011,#19012,#19013,#19014,#19015,
#19016,#19017,#19018,#19019,#19020,#19021,#19022,#19023,#19024,#19025,#19026,
#19027,#19028,#19029,#19030,#19031,#19032,#19033,#19034,#19035,#19036,#19037,
#19038,#19039,#19040,#19041,#19042,#19043,#19044,#19045,#19046,#19047,#19048,
#19049,#19050,#19051,#19052,#19053,#19054,#19055,#19056,#19057,#19058,#19059,
#19060,#19061,#19062,#19063,#19064,#19065,#19066,#19067,#19068,#19069,#19070,
#19071,#19072,#19073,#19074,#19075,#19076,#19077,#19078,#19079,#19080,#19081,
#19082,#19083,#19084,#19085,#19086,#19087,#19088,#19089,#19090,#19091,#19092,
#19093,#19094,#19095,#19096,#19097,#19098,#19099,#19100,#19101,#19102,#19103,
#19104,#19105,#19106,#19107,#19108,#19109,#19110,#19111,#19112,#19113,#19114,
#19115,#19116,#19117,#19118,#19119,#19120,#19121,#19122,#19123,#19124,#19125,
#19126,#19127,#19128,#19129,#19130,#19131,#19132,#19133,#19134,#19135,#19136,
#19137,#19138,#19139,#19140,#19141,#19142,#19143,#19144,#19145,#19146,#19147,
#19148,#19149,#19150,#19151,#19152,#19153,#19154,#19155,#19156,#19157,#19158,
#19159,#19160,#19161,#19162,#19163,#19164,#19165,#19166,#19167,#19168,#19169,
#19170,#19171,#19172,#19173,#19174,#19175,#19176,#19177,#19178,#19179,#19180,
#19181,#19182,#19183),(#19184,#19185,#19186,#19187,#19188,#19189,#19190,
#19191,#19192,#19193,#19194,#19195,#19196,#19197,#19198,#19199,#19200,#19201,
#19202,#19203,#19204,#19205,#19206,#19207,#19208,#19209,#19210,#19211,#19212,
#19213,#19214,#19215,#19216,#19217,#19218,#19219,#19220,#19221,#19222,#19223,
#19224,#19225,#19226,#19227,#19228,#19229,#19230,#19231,#19232,#19233,#19234,
#19235,#19236,#19237,#19238,#19239,#19240,#19241,#19242,#19243,#19244,#19245,
#19246,#19247,#19248,#19249,#19250,#19251,#19252,#19253,#19254,#19255,#19256,
#19257,#19258,#19259,#19260,#19261,#19262,#19263,#19264,#19265,#19266,#19267,
#19268,#19269,#19270,#19271,#19272,#19273,#19274,#19275,#19276,#19277,#19278,
#19279,#19280,#19281,#19282,#19283,#19284,#19285,#19286,#19287,#19288,#19289,
#19290,#19291,#19292,#19293,#19294,#19295,#19296,#19297,#19298,#19299,#19300,
#19301,#19302,#19303,#19304,#19305,#19306,#19307,#19308,#19309,#19310,#19311,
#19312,#19313,#19314,#19315,#19316,#19317,#19318,#19319,#19320,#19321,#19322,
#19323,#19324,#19325,#19326,#19327,#19328,#19329,#19330,#19331,#19332,#19333,
#19334,#19335,#19336,#19337,#19338,#19339,#19340,#19341,#19342,#19343,#19344,
#19345,#19346,#19347,#19348,#19349,#19350,#19351,#19352,#19353,#19354,#19355,
#19356,#19357,#19358,#19359,#19360,#19361,#19362,#19363,#19364,#19365,#19366,
#19367,#19368,#19369,#19370,#19371,#19372,#19373,#19374,#19375,#19376,#19377,
#19378,#19379),(#19380,#19381,#19382,#19383,#19384,#19385,#19386,#19387,
#19388,#19389,#19390,#19391,#19392,#19393,#19394,#19395,#19396,#19397,#19398,
#19399,#19400,#19401,#19402,#19403,#19404,#19405,#19406,#19407,#19408,#19409,
#19410,#19411,#19412,#19413,#19414,#19415,#19416,#19417,#19418,#19419,#19420,
#19421,#19422,#19423,#19424,#19425,#19426,#19427,#19428,#19429,#19430,#19431,
#19432,#19433,#19434,#19435,#19436,#19437,#19438,#19439,#19440,#19441,#19442,
#19443,#19444,#19445,#19446,#19447,#19448,#19449,#19450,#19451,#19452,#19453,
#19454,#19455,#19456,#19457,#19458,#19459,#19460,#19461,#19462,#19463,#19464,
#19465,#19466,#19467,#19468,#19469,#19470,#19471,#19472,#19473,#19474,#19475,
#19476,#19477,#19478,#19479,#19480,#19481,#19482,#19483,#19484,#19485,#19486,
#19487,#19488,#19489,#19490,#19491,#19492,#19493,#19494,#19495,#19496,#19497,
#19498,#19499,#19500,#19501,#19502,#19503,#19504,#19505,#19506,#19507,#19508,
#19509,#19510,#19511,#19512,#19513,#19514,#19515,#19516,#19517,#19518,#19519,
#19520,#19521,#19522,#19523,#19524,#19525,#19526,#19527,#19528,#19529,#19530,
#19531,#19532,#19533,#19534,#19535,#19536,#19537,#19538,#19539,#19540,#19541,
#19542,#19543,#19544,#19545,#19546,#19547,#19548,#19549,#19550,#19551,#19552,
#19553,#19554,#19555,#19556,#19557,#19558,#19559,#19560,#19561,#19562,#19563,
#19564,#19565,#19566,#19567,#19568,#19569,#19570,#19571,#19572,#19573,#19574,
#19575)),.UNSPECIFIED.,.F.,.F.,.F.,(4,4),(4,1,1,1,1,1,1,1,1,1,1,1,1,1,1,
1,1,1,1,1,1,1,1,1,1,1,1,1,1,1,1,1,1,1,1,1,1,1,1,1,1,1,1,1,1,1,1,1,1,1,1,
1,1,1,1,1,1,1,1,1,1,1,1,1,1,1,1,1,1,1,1,1,1,1,1,1,1,1,1,1,1,1,1,1,1,1,1,
1,1,1,1,1,1,1,1,1,1,1,1,1,1,1,1,1,1,1,1,1,1,1,1,1,1,1,1,1,1,1,1,1,1,1,1,
1,1,1,1,1,1,1,1,1,1,1,1,1,1,1,1,1,1,1,1,1,1,1,1,1,1,1,1,1,1,1,1,1,1,1,1,
1,1,1,1,1,1,1,1,1,1,1,1,1,1,1,1,1,1,1,1,1,1,1,1,1,1,1,1,1,1,1,1,1,1,4),
(0.,0.0329955678841871),(11.6159397475006,12.61358260836,13.6112254692194,
14.6088683300789,15.6065111909383,16.6041540517977,17.6017969126571,18.5994397735165,
19.5970826343759,20.5947254952353,21.5923683560947,22.5900112169541,23.5876540778135,
24.5852969386729,25.5829397995323,26.5805826603917,27.5782255212511,28.5758683821105,
29.5735112429699,30.5711541038294,31.5687969646888,32.5664398255482,33.5640826864076,
34.561725547267,35.5593684081264,36.5570112689858,37.5546541298452,38.5522969907046,
39.549939851564,40.5475827124234,41.5452255732828,42.5428684341422,43.5405112950016,
44.538154155861,45.5357970167204,46.5334398775799,47.5310827384393,48.5287255992987,
49.5263684601581,50.5240113210175,51.5216541818769,52.5192970427363,53.5169399035957,
54.5145827644551,55.5122256253145,56.5098684861739,57.5075113470333,58.5051542078927,
59.5027970687521,60.5004399296115,61.4980827904709,62.4957256513303,63.4933685121897,
64.4910113730492,65.4886542339086,66.486297094768,67.4839399556274,68.4815828164868,
69.4792256773462,70.4768685382056,71.474511399065,72.4721542599244,73.4697971207838,
74.4674399816432,75.4650828425026,76.462725703362,77.4603685642214,78.4580114250808,
79.4556542859402,80.4532971467996,81.4509400076591,82.4485828685185,83.4462257293779,
84.4438685902373,85.4415114510967,86.4391543119561,87.4367971728155,88.4344400336749,
89.4320828945343,90.4297257553937,91.4273686162531,92.4250114771125,93.4226543379719,
94.4202971988313,95.4179400596907,96.4155829205502,97.4132257814096,98.410868642269,
99.4085115031284,100.406154363988,101.403797224847,102.401440085707,103.399082946566,
104.396725807425,105.394368668285,106.392011529144,107.389654390004,108.387297250863,
109.384940111722,110.382582972582,111.380225833441,112.377868694301,113.37551155516,
114.373154416019,115.370797276879,116.368440137738,117.366082998598,118.363725859457,
119.361368720316,120.359011581176,121.356654442035,122.354297302895,123.351940163754,
124.349583024614,125.347225885473,126.344868746332,127.342511607192,128.340154468051,
129.337797328911,130.33544018977,131.333083050629,132.330725911489,133.328368772348,
134.326011633208,135.323654494067,136.321297354926,137.318940215786,138.316583076645,
139.314225937505,140.311868798364,141.309511659223,142.307154520083,143.304797380942,
144.302440241802,145.300083102661,146.29772596352,147.29536882438,148.293011685239,
149.290654546099,150.288297406958,151.285940267817,152.283583128677,153.281225989536,
154.278868850396,155.276511711255,156.274154572115,157.271797432974,158.269440293833,
159.267083154693,160.264726015552,161.262368876412,162.260011737271,163.25765459813,
164.25529745899,165.252940319849,166.250583180709,167.248226041568,168.245868902427,
169.243511763287,170.241154624146,171.238797485006,172.236440345865,173.234083206724,
174.231726067584,175.229368928443,176.227011789303,177.224654650162,178.222297511021,
179.219940371881,180.21758323274,181.2152260936,182.212868954459,183.210511815318,
184.208154676178,185.205797537037,186.203440397897,187.201083258756,188.198726119616,
189.196368980475,190.194011841334,191.191654702194,192.189297563053,193.186940423913,
194.184583284772,195.182226145631,196.179869006491,197.17751186735,198.17515472821,
199.172797589069,200.170440449928,201.168083310788,202.165726171647,203.163369032507,
204.161011893366),.UNSPECIFIED.);
#157=B_SPLINE_SURFACE_WITH_KNOTS('',3,3,((#19665,#19666,#19667,#19668,#19669,
#19670,#19671,#19672,#19673,#19674,#19675,#19676,#19677,#19678,#19679,#19680,
#19681,#19682,#19683,#19684,#19685,#19686,#19687,#19688,#19689,#19690,#19691,
#19692,#19693,#19694,#19695,#19696,#19697,#19698,#19699,#19700,#19701,#19702,
#19703,#19704,#19705,#19706,#19707,#19708,#19709,#19710,#19711,#19712,#19713,
#19714,#19715,#19716,#19717,#19718,#19719,#19720,#19721,#19722,#19723,#19724,
#19725,#19726,#19727,#19728,#19729,#19730,#19731,#19732,#19733,#19734,#19735,
#19736,#19737,#19738,#19739,#19740,#19741,#19742,#19743,#19744,#19745,#19746,
#19747,#19748,#19749,#19750,#19751,#19752,#19753,#19754,#19755,#19756,#19757,
#19758,#19759,#19760,#19761,#19762,#19763,#19764,#19765,#19766,#19767,#19768,
#19769,#19770,#19771,#19772,#19773,#19774,#19775,#19776,#19777,#19778,#19779,
#19780,#19781,#19782,#19783,#19784,#19785,#19786,#19787,#19788,#19789,#19790,
#19791,#19792,#19793,#19794,#19795,#19796,#19797,#19798,#19799,#19800,#19801,
#19802,#19803,#19804,#19805,#19806,#19807,#19808,#19809,#19810,#19811,#19812,
#19813,#19814,#19815,#19816,#19817,#19818,#19819,#19820,#19821,#19822,#19823,
#19824,#19825,#19826,#19827,#19828,#19829,#19830,#19831,#19832,#19833,#19834,
#19835,#19836,#19837,#19838,#19839,#19840,#19841,#19842,#19843,#19844,#19845,
#19846,#19847,#19848,#19849,#19850,#19851,#19852,#19853,#19854,#19855,#19856,
#19857,#19858,#19859,#19860,#19861,#19862),(#19863,#19864,#19865,#19866,
#19867,#19868,#19869,#19870,#19871,#19872,#19873,#19874,#19875,#19876,#19877,
#19878,#19879,#19880,#19881,#19882,#19883,#19884,#19885,#19886,#19887,#19888,
#19889,#19890,#19891,#19892,#19893,#19894,#19895,#19896,#19897,#19898,#19899,
#19900,#19901,#19902,#19903,#19904,#19905,#19906,#19907,#19908,#19909,#19910,
#19911,#19912,#19913,#19914,#19915,#19916,#19917,#19918,#19919,#19920,#19921,
#19922,#19923,#19924,#19925,#19926,#19927,#19928,#19929,#19930,#19931,#19932,
#19933,#19934,#19935,#19936,#19937,#19938,#19939,#19940,#19941,#19942,#19943,
#19944,#19945,#19946,#19947,#19948,#19949,#19950,#19951,#19952,#19953,#19954,
#19955,#19956,#19957,#19958,#19959,#19960,#19961,#19962,#19963,#19964,#19965,
#19966,#19967,#19968,#19969,#19970,#19971,#19972,#19973,#19974,#19975,#19976,
#19977,#19978,#19979,#19980,#19981,#19982,#19983,#19984,#19985,#19986,#19987,
#19988,#19989,#19990,#19991,#19992,#19993,#19994,#19995,#19996,#19997,#19998,
#19999,#20000,#20001,#20002,#20003,#20004,#20005,#20006,#20007,#20008,#20009,
#20010,#20011,#20012,#20013,#20014,#20015,#20016,#20017,#20018,#20019,#20020,
#20021,#20022,#20023,#20024,#20025,#20026,#20027,#20028,#20029,#20030,#20031,
#20032,#20033,#20034,#20035,#20036,#20037,#20038,#20039,#20040,#20041,#20042,
#20043,#20044,#20045,#20046,#20047,#20048,#20049,#20050,#20051,#20052,#20053,
#20054,#20055,#20056,#20057,#20058,#20059,#20060),(#20061,#20062,#20063,
#20064,#20065,#20066,#20067,#20068,#20069,#20070,#20071,#20072,#20073,#20074,
#20075,#20076,#20077,#20078,#20079,#20080,#20081,#20082,#20083,#20084,#20085,
#20086,#20087,#20088,#20089,#20090,#20091,#20092,#20093,#20094,#20095,#20096,
#20097,#20098,#20099,#20100,#20101,#20102,#20103,#20104,#20105,#20106,#20107,
#20108,#20109,#20110,#20111,#20112,#20113,#20114,#20115,#20116,#20117,#20118,
#20119,#20120,#20121,#20122,#20123,#20124,#20125,#20126,#20127,#20128,#20129,
#20130,#20131,#20132,#20133,#20134,#20135,#20136,#20137,#20138,#20139,#20140,
#20141,#20142,#20143,#20144,#20145,#20146,#20147,#20148,#20149,#20150,#20151,
#20152,#20153,#20154,#20155,#20156,#20157,#20158,#20159,#20160,#20161,#20162,
#20163,#20164,#20165,#20166,#20167,#20168,#20169,#20170,#20171,#20172,#20173,
#20174,#20175,#20176,#20177,#20178,#20179,#20180,#20181,#20182,#20183,#20184,
#20185,#20186,#20187,#20188,#20189,#20190,#20191,#20192,#20193,#20194,#20195,
#20196,#20197,#20198,#20199,#20200,#20201,#20202,#20203,#20204,#20205,#20206,
#20207,#20208,#20209,#20210,#20211,#20212,#20213,#20214,#20215,#20216,#20217,
#20218,#20219,#20220,#20221,#20222,#20223,#20224,#20225,#20226,#20227,#20228,
#20229,#20230,#20231,#20232,#20233,#20234,#20235,#20236,#20237,#20238,#20239,
#20240,#20241,#20242,#20243,#20244,#20245,#20246,#20247,#20248,#20249,#20250,
#20251,#20252,#20253,#20254,#20255,#20256,#20257,#20258),(#20259,#20260,
#20261,#20262,#20263,#20264,#20265,#20266,#20267,#20268,#20269,#20270,#20271,
#20272,#20273,#20274,#20275,#20276,#20277,#20278,#20279,#20280,#20281,#20282,
#20283,#20284,#20285,#20286,#20287,#20288,#20289,#20290,#20291,#20292,#20293,
#20294,#20295,#20296,#20297,#20298,#20299,#20300,#20301,#20302,#20303,#20304,
#20305,#20306,#20307,#20308,#20309,#20310,#20311,#20312,#20313,#20314,#20315,
#20316,#20317,#20318,#20319,#20320,#20321,#20322,#20323,#20324,#20325,#20326,
#20327,#20328,#20329,#20330,#20331,#20332,#20333,#20334,#20335,#20336,#20337,
#20338,#20339,#20340,#20341,#20342,#20343,#20344,#20345,#20346,#20347,#20348,
#20349,#20350,#20351,#20352,#20353,#20354,#20355,#20356,#20357,#20358,#20359,
#20360,#20361,#20362,#20363,#20364,#20365,#20366,#20367,#20368,#20369,#20370,
#20371,#20372,#20373,#20374,#20375,#20376,#20377,#20378,#20379,#20380,#20381,
#20382,#20383,#20384,#20385,#20386,#20387,#20388,#20389,#20390,#20391,#20392,
#20393,#20394,#20395,#20396,#20397,#20398,#20399,#20400,#20401,#20402,#20403,
#20404,#20405,#20406,#20407,#20408,#20409,#20410,#20411,#20412,#20413,#20414,
#20415,#20416,#20417,#20418,#20419,#20420,#20421,#20422,#20423,#20424,#20425,
#20426,#20427,#20428,#20429,#20430,#20431,#20432,#20433,#20434,#20435,#20436,
#20437,#20438,#20439,#20440,#20441,#20442,#20443,#20444,#20445,#20446,#20447,
#20448,#20449,#20450,#20451,#20452,#20453,#20454,#20455,#20456)),
 .UNSPECIFIED.,.F.,.F.,.F.,(4,4),(4,1,1,1,1,1,1,1,1,1,1,1,1,1,1,1,1,1,1,
1,1,1,1,1,1,1,1,1,1,1,1,1,1,1,1,1,1,1,1,1,1,1,1,1,1,1,1,1,1,1,1,1,1,1,1,
1,1,1,1,1,1,1,1,1,1,1,1,1,1,1,1,1,1,1,1,1,1,1,1,1,1,1,1,1,1,1,1,1,1,1,1,
1,1,1,1,1,1,1,1,1,1,1,1,1,1,1,1,1,1,1,1,1,1,1,1,1,1,1,1,1,1,1,1,1,1,1,1,
1,1,1,1,1,1,1,1,1,1,1,1,1,1,1,1,1,1,1,1,1,1,1,1,1,1,1,1,1,1,1,1,1,1,1,1,
1,1,1,1,1,1,1,1,1,1,1,1,1,1,1,1,1,1,1,1,1,1,1,1,1,1,1,1,1,1,1,1,4),(0.,
0.0329955678841871),(8.30203615430855,9.30007843543257,10.2981207165566,
11.2961629976806,12.2942052788047,13.2922475599287,14.2902898410527,15.2883321221767,
16.2863744033008,17.2844166844248,18.2824589655488,19.2805012466728,20.2785435277969,
21.2765858089209,22.2746280900449,23.272670371169,24.270712652293,25.268754933417,
26.266797214541,27.2648394956651,28.2628817767891,29.2609240579131,30.2589663390371,
31.2570086201612,32.2550509012852,33.2530931824092,34.2511354635333,35.2491777446573,
36.2472200257813,37.2452623069053,38.2433045880294,39.2413468691534,40.2393891502774,
41.2374314314014,42.2354737125255,43.2335159936495,44.2315582747735,45.2296005558975,
46.2276428370216,47.2256851181456,48.2237273992696,49.2217696803937,50.2198119615177,
51.2178542426417,52.2158965237657,53.2139388048898,54.2119810860138,55.2100233671378,
56.2080656482619,57.2061079293859,58.2041502105099,59.2021924916339,60.200234772758,
61.198277053882,62.196319335006,63.19436161613,64.1924038972541,65.1904461783781,
66.1884884595021,67.1865307406262,68.1845730217502,69.1826153028742,70.1806575839982,
71.1786998651223,72.1767421462463,73.1747844273703,74.1728267084943,75.1708689896184,
76.1689112707424,77.1669535518664,78.1649958329905,79.1630381141145,80.1610803952385,
81.1591226763625,82.1571649574865,83.1552072386106,84.1532495197346,85.1512918008586,
86.1493340819827,87.1473763631067,88.1454186442307,89.1434609253548,90.1415032064788,
91.1395454876028,92.1375877687268,93.1356300498508,94.1336723309749,95.1317146120989,
96.1297568932229,97.127799174347,98.125841455471,99.123883736595,100.121926017719,
101.119968298843,102.118010579967,103.116052861091,104.114095142215,105.112137423339,
106.110179704463,107.108221985587,108.106264266711,109.104306547835,110.102348828959,
111.100391110083,112.098433391207,113.096475672331,114.094517953455,115.092560234579,
116.090602515703,117.088644796828,118.086687077952,119.084729359076,120.0827716402,
121.080813921324,122.078856202448,123.076898483572,124.074940764696,125.07298304582,
126.071025326944,127.069067608068,128.067109889192,129.065152170316,130.06319445144,
131.061236732564,132.059279013688,133.057321294812,134.055363575936,135.05340585706,
136.051448138184,137.049490419308,138.047532700432,139.045574981556,140.04361726268,
141.041659543804,142.039701824928,143.037744106052,144.035786387176,145.0338286683,
146.031870949424,147.029913230548,148.027955511672,149.025997792796,150.02404007392,
151.022082355044,152.020124636168,153.018166917292,154.016209198417,155.014251479541,
156.012293760665,157.010336041789,158.008378322913,159.006420604037,160.004462885161,
161.002505166285,162.000547447409,162.998589728533,163.996632009657,164.994674290781,
165.992716571905,166.990758853029,167.988801134153,168.986843415277,169.984885696401,
170.982927977525,171.980970258649,172.979012539773,173.977054820897,174.975097102021,
175.973139383145,176.971181664269,177.969223945393,178.967266226517,179.965308507641,
180.963350788765,181.961393069889,182.959435351013,183.957477632137,184.955519913261,
185.953562194385,186.951604475509,187.949646756633,188.947689037757,189.945731318881,
190.943773600006,191.94181588113,192.939858162254,193.937900443378,194.935942724502,
195.933985005626,196.93202728675,197.930069567874,198.928111848998,199.926154130122,
200.924196411246,201.92223869237,202.920280973494),.UNSPECIFIED.);
#158=B_SPLINE_SURFACE_WITH_KNOTS('',3,3,((#20915,#20916,#20917,#20918,#20919,
#20920,#20921,#20922,#20923,#20924,#20925,#20926,#20927,#20928,#20929,#20930,
#20931,#20932,#20933,#20934,#20935,#20936,#20937,#20938,#20939,#20940,#20941,
#20942,#20943,#20944,#20945,#20946,#20947,#20948,#20949,#20950),(#20951,
#20952,#20953,#20954,#20955,#20956,#20957,#20958,#20959,#20960,#20961,#20962,
#20963,#20964,#20965,#20966,#20967,#20968,#20969,#20970,#20971,#20972,#20973,
#20974,#20975,#20976,#20977,#20978,#20979,#20980,#20981,#20982,#20983,#20984,
#20985,#20986),(#20987,#20988,#20989,#20990,#20991,#20992,#20993,#20994,
#20995,#20996,#20997,#20998,#20999,#21000,#21001,#21002,#21003,#21004,#21005,
#21006,#21007,#21008,#21009,#21010,#21011,#21012,#21013,#21014,#21015,#21016,
#21017,#21018,#21019,#21020,#21021,#21022),(#21023,#21024,#21025,#21026,
#21027,#21028,#21029,#21030,#21031,#21032,#21033,#21034,#21035,#21036,#21037,
#21038,#21039,#21040,#21041,#21042,#21043,#21044,#21045,#21046,#21047,#21048,
#21049,#21050,#21051,#21052,#21053,#21054,#21055,#21056,#21057,#21058)),
 .UNSPECIFIED.,.F.,.F.,.F.,(4,4),(4,1,1,1,1,1,1,1,1,1,1,1,1,1,1,1,1,1,1,
1,1,1,1,1,1,1,1,1,1,1,1,1,1,4),(0.,0.0321584099938622),(11.8553612635794,
12.830508595889,13.8056559281987,14.7808032605084,15.755950592818,16.7310979251277,
17.7062452574374,18.681392589747,19.6565399220567,20.6316872543664,21.606834586676,
22.5819819189857,23.5571292512954,24.532276583605,25.5074239159147,26.4825712482243,
27.457718580534,28.4328659128437,29.4080132451533,30.383160577463,31.3583079097727,
32.3334552420823,33.308602574392,34.2837499067017,35.2588972390113,36.234044571321,
37.2091919036307,38.1843392359403,39.15948656825,40.1346339005596,41.1097812328693,
42.084928565179,43.0600758974886,44.0352232297983),.UNSPECIFIED.);
#159=B_SPLINE_SURFACE_WITH_KNOTS('',3,3,((#21182,#21183,#21184,#21185,#21186,
#21187,#21188,#21189,#21190,#21191,#21192,#21193,#21194,#21195,#21196,#21197,
#21198,#21199,#21200,#21201,#21202,#21203,#21204,#21205,#21206,#21207,#21208,
#21209,#21210,#21211,#21212,#21213,#21214,#21215,#21216,#21217),(#21218,
#21219,#21220,#21221,#21222,#21223,#21224,#21225,#21226,#21227,#21228,#21229,
#21230,#21231,#21232,#21233,#21234,#21235,#21236,#21237,#21238,#21239,#21240,
#21241,#21242,#21243,#21244,#21245,#21246,#21247,#21248,#21249,#21250,#21251,
#21252,#21253),(#21254,#21255,#21256,#21257,#21258,#21259,#21260,#21261,
#21262,#21263,#21264,#21265,#21266,#21267,#21268,#21269,#21270,#21271,#21272,
#21273,#21274,#21275,#21276,#21277,#21278,#21279,#21280,#21281,#21282,#21283,
#21284,#21285,#21286,#21287,#21288,#21289),(#21290,#21291,#21292,#21293,
#21294,#21295,#21296,#21297,#21298,#21299,#21300,#21301,#21302,#21303,#21304,
#21305,#21306,#21307,#21308,#21309,#21310,#21311,#21312,#21313,#21314,#21315,
#21316,#21317,#21318,#21319,#21320,#21321,#21322,#21323,#21324,#21325)),
 .UNSPECIFIED.,.F.,.F.,.F.,(4,4),(4,1,1,1,1,1,1,1,1,1,1,1,1,1,1,1,1,1,1,
1,1,1,1,1,1,1,1,1,1,1,1,1,1,4),(0.,0.0321584099938622),(14.3984001269719,
15.3735474592815,16.3486947915912,17.3238421239009,18.2989894562105,19.2741367885202,
20.2492841208299,21.2244314531395,22.1995787854492,23.1747261177589,24.1498734500685,
25.1250207823782,26.1001681146879,27.0753154469975,28.0504627793072,29.0256101116168,
30.0007574439265,30.9759047762362,31.9510521085458,32.9261994408555,33.9013467731652,
34.8764941054748,35.8516414377845,36.8267887700942,37.8019361024038,38.7770834347135,
39.7522307670232,40.7273780993328,41.7025254316425,42.6776727639522,43.6528200962618,
44.6279674285715,45.6031147608811,46.5782620931908),.UNSPECIFIED.);
#160=B_SPLINE_SURFACE_WITH_KNOTS('',3,3,((#21557,#21558,#21559,#21560,#21561),
(#21562,#21563,#21564,#21565,#21566),(#21567,#21568,#21569,#21570,#21571),
(#21572,#21573,#21574,#21575,#21576),(#21577,#21578,#21579,#21580,#21581)),
 .UNSPECIFIED.,.F.,.F.,.F.,(4,1,4),(4,1,4),(0.,0.571428571428571,1.),(0.,
0.0453052401185593,0.105712226943305),.UNSPECIFIED.);
#161=B_SPLINE_SURFACE_WITH_KNOTS('',3,3,((#21604,#21605,#21606,#21607,#21608),
(#21609,#21610,#21611,#21612,#21613),(#21614,#21615,#21616,#21617,#21618),
(#21619,#21620,#21621,#21622,#21623),(#21624,#21625,#21626,#21627,#21628)),
 .UNSPECIFIED.,.F.,.F.,.F.,(4,1,4),(4,1,4),(0.,0.571428571428571,1.),(0.,
0.0453052401439183,0.105712227002476),.UNSPECIFIED.);
#162=B_SPLINE_SURFACE_WITH_KNOTS('',3,3,((#21642,#21643,#21644,#21645,#21646),
(#21647,#21648,#21649,#21650,#21651),(#21652,#21653,#21654,#21655,#21656),
(#21657,#21658,#21659,#21660,#21661),(#21662,#21663,#21664,#21665,#21666)),
 .UNSPECIFIED.,.F.,.F.,.F.,(4,1,4),(4,1,4),(0.,0.571428571428571,1.),(0.,
4.20509945658767,9.8118987320379),.UNSPECIFIED.);
#163=B_SPLINE_SURFACE_WITH_KNOTS('',3,3,((#21680,#21681,#21682,#21683,#21684),
(#21685,#21686,#21687,#21688,#21689),(#21690,#21691,#21692,#21693,#21694),
(#21695,#21696,#21697,#21698,#21699),(#21700,#21701,#21702,#21703,#21704)),
 .UNSPECIFIED.,.F.,.F.,.F.,(4,1,4),(4,1,4),(0.,0.571428571428571,1.),(0.,
0.0444882141544403,0.103805833027027),.UNSPECIFIED.);
#164=B_SPLINE_SURFACE_WITH_KNOTS('',3,3,((#21724,#21725,#21726,#21727,#21728),
(#21729,#21730,#21731,#21732,#21733),(#21734,#21735,#21736,#21737,#21738),
(#21739,#21740,#21741,#21742,#21743),(#21744,#21745,#21746,#21747,#21748)),
 .UNSPECIFIED.,.F.,.F.,.F.,(4,1,4),(4,1,4),(0.,0.571428571428571,1.),(2.06005858395869E-18,
0.0444882141931362,0.103805833117318),.UNSPECIFIED.);
#165=B_SPLINE_SURFACE_WITH_KNOTS('',3,3,((#21762,#21763,#21764,#21765,#21766),
(#21767,#21768,#21769,#21770,#21771),(#21772,#21773,#21774,#21775,#21776),
(#21777,#21778,#21779,#21780,#21781),(#21782,#21783,#21784,#21785,#21786)),
 .UNSPECIFIED.,.F.,.F.,.F.,(4,1,4),(4,1,4),(0.,0.571428571428571,1.),(0.,
4.20509909783593,9.81189789495051),.UNSPECIFIED.);
#166=B_SPLINE_SURFACE_WITH_KNOTS('',3,3,((#21809,#21810,#21811,#21812),
(#21813,#21814,#21815,#21816),(#21817,#21818,#21819,#21820),(#21821,#21822,
#21823,#21824),(#21825,#21826,#21827,#21828)),.UNSPECIFIED.,.F.,.F.,.F.,
(4,1,4),(4,4),(0.,0.571428571428571,1.),(-0.00268702576369722,0.125151053668407),
 .UNSPECIFIED.);
#167=B_SPLINE_SURFACE_WITH_KNOTS('',3,3,((#21862,#21863,#21864,#21865),
(#21866,#21867,#21868,#21869),(#21870,#21871,#21872,#21873),(#21874,#21875,
#21876,#21877)),.UNSPECIFIED.,.F.,.F.,.F.,(4,4),(4,4),(0.0135518988075539,
0.986045335056424),(0.,0.622596671418298),.UNSPECIFIED.);
#168=B_SPLINE_SURFACE_WITH_KNOTS('',3,3,((#21887,#21888,#21889,#21890),
(#21891,#21892,#21893,#21894),(#21895,#21896,#21897,#21898),(#21899,#21900,
#21901,#21902),(#21903,#21904,#21905,#21906)),.UNSPECIFIED.,.F.,.F.,.F.,
(4,1,4),(4,4),(0.,0.571428571428571,1.),(-0.00281084541253883,0.124959300034279),
 .UNSPECIFIED.);
#169=B_SPLINE_SURFACE_WITH_KNOTS('',3,3,((#21948,#21949,#21950,#21951),
(#21952,#21953,#21954,#21955),(#21956,#21957,#21958,#21959),(#21960,#21961,
#21962,#21963),(#21964,#21965,#21966,#21967)),.UNSPECIFIED.,.F.,.F.,.F.,
(4,1,4),(4,4),(0.,0.571428571428571,1.),(-0.00261432509268751,0.125151053668407),
 .UNSPECIFIED.);
#170=B_SPLINE_SURFACE_WITH_KNOTS('',3,3,((#22001,#22002,#22003,#22004),
(#22005,#22006,#22007,#22008),(#22009,#22010,#22011,#22012),(#22013,#22014,
#22015,#22016),(#22017,#22018,#22019,#22020)),.UNSPECIFIED.,.F.,.F.,.F.,
(4,1,4),(4,4),(0.,0.571428571428571,1.),(-0.00286362952972032,0.12495930003428),
 .UNSPECIFIED.);
#171=B_SPLINE_SURFACE_WITH_KNOTS('',3,3,((#22059,#22060,#22061,#22062),
(#22063,#22064,#22065,#22066),(#22067,#22068,#22069,#22070),(#22071,#22072,
#22073,#22074)),.UNSPECIFIED.,.F.,.F.,.F.,(4,4),(4,4),(0.0139546649435754,
0.986448101192446),(0.,0.622596671418299),.UNSPECIFIED.);
#172=B_SPLINE_CURVE_WITH_KNOTS('',3,(#12264,#12265,#12266,#12267,#12268,
#12269,#12270,#12271,#12272,#12273,#12274,#12275,#12276,#12277,#12278,#12279,
#12280,#12281,#12282,#12283,#12284,#12285,#12286,#12287),.UNSPECIFIED.,
 .F.,.F.,(4,2,2,2,2,2,2,2,2,2,2,4),(-0.337265338267783,-0.250544943628509,
-0.208272806508042,-0.186542211788094,-0.176382978682897,-0.170925844043069,
-0.16639450677335,-0.161077381235501,-0.15182241135393,-0.115009181549223,
-0.030206004227969,0.),.UNSPECIFIED.);
#173=B_SPLINE_CURVE_WITH_KNOTS('',3,(#12292,#12293,#12294,#12295,#12296,
#12297,#12298,#12299,#12300,#12301,#12302,#12303,#12304,#12305,#12306,#12307,
#12308,#12309,#12310,#12311),.UNSPECIFIED.,.F.,.F.,(4,2,2,2,2,2,2,2,2,4),
(-0.240982594686416,-0.16829976149504,-0.141836598208813,-0.129116059226128,
-0.121962912034391,-0.115857591426886,-0.108506552485159,-0.0948769875819265,
-0.0364654790774683,0.),.UNSPECIFIED.);
#174=B_SPLINE_CURVE_WITH_KNOTS('',3,(#12316,#12317,#12318,#12319,#12320,
#12321,#12322,#12323,#12324,#12325,#12326,#12327,#12328,#12329,#12330,#12331,
#12332,#12333,#12334,#12335),.UNSPECIFIED.,.F.,.F.,(4,2,2,2,2,2,2,2,2,4),
(-0.240981214998207,-0.168303541671295,-0.141841407502325,-0.129121097580905,
-0.121968013294536,-0.115862708924237,-0.108511643765797,-0.0948818976588229,
-0.0364681276985956,0.),.UNSPECIFIED.);
#175=B_SPLINE_CURVE_WITH_KNOTS('',3,(#12340,#12341,#12342,#12343,#12344,
#12345,#12346,#12347,#12348,#12349,#12350,#12351,#12352,#12353,#12354,#12355,
#12356,#12357,#12358,#12359,#12360,#12361,#12362,#12363),.UNSPECIFIED.,
 .F.,.F.,(4,2,2,2,2,2,2,2,2,2,2,4),(-0.337269388373684,-0.250545316912909,
-0.208282401844766,-0.186554569827561,-0.176396213396297,-0.17093921790305,
-0.16640782243471,-0.161090427650893,-0.151834477986603,-0.115010808423941,
-0.0302102096065556,0.),.UNSPECIFIED.);
#176=B_SPLINE_CURVE_WITH_KNOTS('',3,(#12386,#12387,#12388,#12389),
 .UNSPECIFIED.,.F.,.F.,(4,4),(1.0454440030657,2.52465537163019),
 .UNSPECIFIED.);
#177=B_SPLINE_CURVE_WITH_KNOTS('',3,(#12391,#12392,#12393,#12394,#12395,
#12396,#12397,#12398,#12399,#12400,#12401,#12402,#12403,#12404,#12405,#12406,
#12407,#12408,#12409,#12410,#12411,#12412,#12413,#12414,#12415,#12416,#12417,
#12418),.UNSPECIFIED.,.F.,.F.,(4,3,3,3,3,3,3,3,3,4),(-0.152193408756968,
-0.128427023368412,-0.115107736263918,-0.0911810900745799,-0.0780377802127556,
-0.0652031397886901,-0.0414031558437525,-0.0389949527774582,-0.0152076153333754,
0.),.UNSPECIFIED.);
#178=B_SPLINE_CURVE_WITH_KNOTS('',3,(#12420,#12421,#12422,#12423),
 .UNSPECIFIED.,.F.,.F.,(4,4),(-3.44967454744645,-1.05170160817356),
 .UNSPECIFIED.);
#179=B_SPLINE_CURVE_WITH_KNOTS('',3,(#12425,#12426,#12427,#12428,#12429,
#12430,#12431,#12432,#12433,#12434,#12435,#12436,#12437,#12438,#12439,#12440,
#12441,#12442,#12443,#12444,#12445,#12446,#12447,#12448,#12449,#12450,#12451,
#12452),.UNSPECIFIED.,.F.,.F.,(4,3,3,3,3,3,3,3,3,4),(-0.152278960443096,
-0.128503570101575,-0.115218572146868,-0.09145408274965,-0.0870214650669139,
-0.0781562978024333,-0.0542566895399357,-0.03908030849237,-0.0153296112319379,
0.),.UNSPECIFIED.);
#180=B_SPLINE_CURVE_WITH_KNOTS('',3,(#12453,#12454,#12455,#12456),
 .UNSPECIFIED.,.F.,.F.,(4,4),(2.75501813708031,3.4476340663212),
 .UNSPECIFIED.);
#181=B_SPLINE_CURVE_WITH_KNOTS('',3,(#12478,#12479,#12480,#12481),
 .UNSPECIFIED.,.F.,.F.,(4,4),(7.24810383506675,7.89761558728778),
 .UNSPECIFIED.);
#182=B_SPLINE_CURVE_WITH_KNOTS('',3,(#12483,#12484,#12485,#12486,#12487,
#12488,#12489,#12490,#12491,#12492,#12493,#12494,#12495,#12496,#12497,#12498,
#12499,#12500,#12501,#12502,#12503,#12504,#12505,#12506,#12507,#12508,#12509,
#12510),.UNSPECIFIED.,.F.,.F.,(4,3,3,3,3,3,3,3,3,4),(-0.152278869104567,
-0.128548794904564,-0.115192257893812,-0.0912773536606376,-0.0781090575823055,
-0.0652724057916263,-0.0414819581560496,-0.0390493575290778,-0.015259721743698,
0.),.UNSPECIFIED.);
#183=B_SPLINE_CURVE_WITH_KNOTS('',3,(#12512,#12513,#12514,#12515),
 .UNSPECIFIED.,.F.,.F.,(4,4),(-9.94532343034734,-7.24519303641511),
 .UNSPECIFIED.);
#184=B_SPLINE_CURVE_WITH_KNOTS('',3,(#12517,#12518,#12519,#12520,#12521,
#12522,#12523,#12524,#12525,#12526,#12527,#12528,#12529,#12530,#12531,#12532,
#12533,#12534,#12535,#12536,#12537,#12538,#12539,#12540,#12541,#12542,#12543,
#12544),.UNSPECIFIED.,.F.,.F.,(4,3,3,3,3,3,3,3,3,4),(-0.152181623618259,
-0.128410404494075,-0.115248188224843,-0.0914746846046984,-0.0869904866333268,
-0.0783028696190655,-0.0543945376065823,-0.0391651209697638,-0.0153884182770307,
0.),.UNSPECIFIED.);
#185=B_SPLINE_CURVE_WITH_KNOTS('',3,(#12545,#12546,#12547,#12548),
 .UNSPECIFIED.,.F.,.F.,(4,4),(8.21380824320284,9.95046871680089),
 .UNSPECIFIED.);
#186=B_SPLINE_CURVE_WITH_KNOTS('',3,(#12551,#12552,#12553,#12554),
 .UNSPECIFIED.,.F.,.F.,(4,4),(2.80491490332713,3.45442665446657),
 .UNSPECIFIED.);
#187=B_SPLINE_CURVE_WITH_KNOTS('',3,(#12558,#12559,#12560,#12561),
 .UNSPECIFIED.,.F.,.F.,(4,4),(0.752061768057538,2.48872224644044),
 .UNSPECIFIED.);
#188=B_SPLINE_CURVE_WITH_KNOTS('',3,(#12709,#12710,#12711,#12712,#12713,
#12714),.UNSPECIFIED.,.F.,.F.,(4,2,4),(-0.606700505977711,-0.303383635264422,
-0.000339350725729326),.UNSPECIFIED.);
#189=B_SPLINE_CURVE_WITH_KNOTS('',3,(#12715,#12716,#12717,#12718,#12719,
#12720,#12721,#12722,#12723,#12724,#12725,#12726,#12727,#12728,#12729,#12730,
#12731,#12732,#12733,#12734,#12735,#12736,#12737,#12738,#12739,#12740,#12741,
#12742),.UNSPECIFIED.,.F.,.F.,(4,3,3,3,3,3,3,3,3,4),(-0.152173579228948,
-0.128423230539522,-0.115115104157663,-0.0911927259648815,-0.0780672068328041,
-0.0652082609452843,-0.0414117413801899,-0.0390174000215468,-0.0152300060615686,
0.),.UNSPECIFIED.);
#190=B_SPLINE_CURVE_WITH_KNOTS('',3,(#12743,#12744,#12745,#12746,#12747,
#12748),.UNSPECIFIED.,.F.,.F.,(4,2,4),(-0.606471894652381,-0.303383500305553,
-0.00011071898471493),.UNSPECIFIED.);
#191=B_SPLINE_CURVE_WITH_KNOTS('',3,(#12752,#12753,#12754,#12755,#12756,
#12757),.UNSPECIFIED.,.F.,.F.,(4,2,4),(-0.606240625011114,-0.303433113375332,
-0.00010938105916114),.UNSPECIFIED.);
#192=B_SPLINE_CURVE_WITH_KNOTS('',3,(#12759,#12760,#12761,#12762,#12763,
#12764,#12765,#12766,#12767,#12768,#12769,#12770,#12771,#12772,#12773,#12774,
#12775,#12776,#12777,#12778,#12779,#12780,#12781,#12782,#12783,#12784,#12785,
#12786),.UNSPECIFIED.,.F.,.F.,(4,3,3,3,3,3,3,3,3,4),(-0.152281454644235,
-0.128508102092242,-0.115234945630277,-0.0914677943501604,-0.0870276017853555,
-0.0781846052914712,-0.0542821334115454,-0.0390966859411886,-0.0153419673568312,
0.),.UNSPECIFIED.);
#193=B_SPLINE_CURVE_WITH_KNOTS('',3,(#12788,#12789,#12790,#12791,#12792,
#12793),.UNSPECIFIED.,.F.,.F.,(4,2,4),(-0.606758573154242,-0.303433157101101,
-0.000627306481538803),.UNSPECIFIED.);
#194=B_SPLINE_CURVE_WITH_KNOTS('',3,(#12799,#12800,#12801,#12802,#12803,
#12804),.UNSPECIFIED.,.F.,.F.,(4,2,4),(-0.60617382748,-0.303436117212405,
-7.2700296824213E-5),.UNSPECIFIED.);
#195=B_SPLINE_CURVE_WITH_KNOTS('',3,(#12806,#12807,#12808,#12809,#12810,
#12811,#12812,#12813,#12814,#12815,#12816,#12817,#12818,#12819,#12820,#12821,
#12822,#12823,#12824,#12825,#12826,#12827,#12828,#12829,#12830,#12831,#12832,
#12833),.UNSPECIFIED.,.F.,.F.,(4,3,3,3,3,3,3,3,3,4),(-0.152282154327755,
-0.128558036203745,-0.115201429639692,-0.0912891813973639,-0.0781219052297615,
-0.065279687589213,-0.0414913146723999,-0.0390591331507366,-0.0152683745546824,
0.),.UNSPECIFIED.);
#196=B_SPLINE_CURVE_WITH_KNOTS('',3,(#12837,#12838,#12839,#12840,#12841,
#12842,#12843,#12844,#12845,#12846,#12847,#12848,#12849,#12850,#12851,#12852,
#12853,#12854,#12855,#12856,#12857,#12858,#12859,#12860,#12861,#12862,#12863,
#12864),.UNSPECIFIED.,.F.,.F.,(4,3,3,3,3,3,3,3,3,4),(-0.152283066055976,
-0.128508717930245,-0.115216472798554,-0.091451700383826,-0.087022506454752,
-0.0781485278686168,-0.0542483994686567,-0.0390758108455304,-0.0153274175274101,
0.),.UNSPECIFIED.);
#197=B_SPLINE_CURVE_WITH_KNOTS('',3,(#12866,#12867,#12868,#12869,#12870,
#12871),.UNSPECIFIED.,.F.,.F.,(4,2,4),(-0.606800264911061,-0.303436147592132,
-0.000699137727853738),.UNSPECIFIED.);
#198=B_SPLINE_CURVE_WITH_KNOTS('',3,(#12876,#12877,#12878,#12879,#12880,
#12881),.UNSPECIFIED.,.F.,.F.,(4,2,4),(-0.606915279655722,-0.30363236403835,
-0.000516487074480598),.UNSPECIFIED.);
#199=B_SPLINE_CURVE_WITH_KNOTS('',3,(#12885,#12886,#12887,#12888,#12889,
#12890,#12891,#12892,#12893,#12894,#12895,#12896,#12897,#12898,#12899,#12900,
#12901,#12902,#12903,#12904,#12905,#12906,#12907,#12908,#12909,#12910,#12911,
#12912),.UNSPECIFIED.,.F.,.F.,(4,3,3,3,3,3,3,3,3,4),(-0.152205325335401,
-0.128433618138404,-0.115304790388008,-0.091527299141506,-0.0870178586418932,
-0.0783866443643876,-0.0544751548276533,-0.0392137310602028,-0.0154203878854647,
0.),.UNSPECIFIED.);
#200=B_SPLINE_CURVE_WITH_KNOTS('',3,(#12914,#12915,#12916,#12917,#12918,
#12919),.UNSPECIFIED.,.F.,.F.,(4,2,4),(-0.606752424187958,-0.303632696349781,
-0.000353591088346872),.UNSPECIFIED.);
#201=B_SPLINE_CURVE_WITH_KNOTS('',3,(#12925,#12926,#12927,#12928),
 .UNSPECIFIED.,.F.,.F.,(4,4),(0.0116023361771303,0.618489359031386),
 .UNSPECIFIED.);
#202=B_SPLINE_CURVE_WITH_KNOTS('',3,(#12932,#12933,#12934,#12935),
 .UNSPECIFIED.,.F.,.F.,(4,4),(-0.618489359031386,-0.01160233617713),
 .UNSPECIFIED.);
#203=B_SPLINE_CURVE_WITH_KNOTS('',3,(#12938,#12939,#12940,#12941),
 .UNSPECIFIED.,.F.,.F.,(4,4),(7.01593971618694,9.71770560667459),
 .UNSPECIFIED.);
#204=B_SPLINE_CURVE_WITH_KNOTS('',3,(#12942,#12943,#12944,#12945),
 .UNSPECIFIED.,.F.,.F.,(4,4),(0.505945342046796,3.20718651982575),
 .UNSPECIFIED.);
#205=B_SPLINE_CURVE_WITH_KNOTS('',3,(#12948,#12949,#12950,#12951,#12952,
#12953,#12954),.UNSPECIFIED.,.F.,.F.,(4,3,4),(3.40717417387402,5.11170895874517,
6.80746068626633),.UNSPECIFIED.);
#206=B_SPLINE_CURVE_WITH_KNOTS('',3,(#12957,#12958,#12959,#12960),
 .UNSPECIFIED.,.F.,.F.,(4,4),(7.00766573366377,9.41198845520559),
 .UNSPECIFIED.);
#207=B_SPLINE_CURVE_WITH_KNOTS('',3,(#12964,#12965,#12966,#12967),
 .UNSPECIFIED.,.F.,.F.,(4,4),(9.61248784142317,10.2217363065808),
 .UNSPECIFIED.);
#208=B_SPLINE_CURVE_WITH_KNOTS('',3,(#12968,#12969,#12970,#12971,#12972,
#12973,#12974,#12975,#12976,#12977,#12978,#12979,#12980,#12981,#12982,#12983,
#12984,#12985,#12986,#12987,#12988,#12989,#12990,#12991,#12992,#12993,#12994,
#12995),.UNSPECIFIED.,.F.,.F.,(4,3,3,3,3,3,3,3,3,4),(0.,0.0238103109064959,
0.0390781362249314,0.0628635086275546,0.0641230352384255,0.0780643700703951,
0.101962174814111,0.113803522271848,0.137549611554782,0.149564734365165),
 .UNSPECIFIED.);
#209=B_SPLINE_CURVE_WITH_KNOTS('',3,(#12999,#13000,#13001,#13002,#13003,
#13004,#13005,#13006,#13007,#13008,#13009,#13010,#13011,#13012,#13013,#13014,
#13015,#13016,#13017,#13018,#13019,#13020,#13021,#13022,#13023,#13024,#13025,
#13026,#13027,#13028,#13029),.UNSPECIFIED.,.F.,.F.,(4,3,3,3,3,3,3,3,3,3,
4),(0.,0.0535521515156599,0.107729685495911,0.117233338918226,0.171447998942947,
0.1923696899792,0.234191611538245,0.288659693466396,0.341410301570312,0.395549383747909,
0.448696573746633),.UNSPECIFIED.);
#210=B_SPLINE_CURVE_WITH_KNOTS('',3,(#13031,#13032,#13033,#13034),
 .UNSPECIFIED.,.F.,.F.,(4,4),(0.0255858263485814,0.973760737485873),
 .UNSPECIFIED.);
#211=B_SPLINE_CURVE_WITH_KNOTS('',3,(#13036,#13037,#13038,#13039,#13040,
#13041,#13042,#13043,#13044,#13045,#13046,#13047,#13048,#13049,#13050,#13051,
#13052,#13053,#13054,#13055,#13056,#13057,#13058,#13059,#13060,#13061,#13062,
#13063,#13064,#13065,#13066),.UNSPECIFIED.,.F.,.F.,(4,3,3,3,3,3,3,3,3,3,
4),(0.,0.0535144560117858,0.107726856902975,0.117300577410231,0.171517675930231,
0.195438847090422,0.234297456941738,0.289665153342662,0.345032849743585,
0.40043206955427,0.455831289364955),.UNSPECIFIED.);
#212=B_SPLINE_CURVE_WITH_KNOTS('',3,(#13070,#13071,#13072,#13073,#13074,
#13075,#13076,#13077,#13078,#13079,#13080,#13081,#13082,#13083,#13084,#13085,
#13086,#13087,#13088,#13089,#13090,#13091,#13092,#13093,#13094,#13095,#13096,
#13097,#13098,#13099,#13100),.UNSPECIFIED.,.F.,.F.,(4,3,3,3,3,3,3,3,3,3,
4),(0.,0.053505543180391,0.107714168832353,0.117253997025819,0.171473395203321,
0.195418854185489,0.234223199196375,0.289607016015183,0.344990832833991,
0.400409777473312,0.455828722112633),.UNSPECIFIED.);
#213=B_SPLINE_CURVE_WITH_KNOTS('',3,(#13102,#13103,#13104,#13105),
 .UNSPECIFIED.,.F.,.F.,(4,4),(0.0262392625141271,0.974414173651419),
 .UNSPECIFIED.);
#214=B_SPLINE_CURVE_WITH_KNOTS('',3,(#13107,#13108,#13109,#13110,#13111,
#13112,#13113,#13114,#13115,#13116,#13117,#13118,#13119,#13120,#13121,#13122,
#13123,#13124,#13125,#13126,#13127,#13128,#13129,#13130,#13131,#13132,#13133,
#13134,#13135,#13136,#13137),.UNSPECIFIED.,.F.,.F.,(4,3,3,3,3,3,3,3,3,3,
4),(0.,0.0535648734523888,0.107747221190676,0.117299947751206,0.171510987106922,
0.192397607227928,0.234296687348373,0.288768001369001,0.341469499352622,
0.395597672314973,0.448700135162036),.UNSPECIFIED.);
#215=B_SPLINE_CURVE_WITH_KNOTS('',3,(#13140,#13141,#13142,#13143,#13144,
#13145,#13146,#13147,#13148,#13149,#13150,#13151,#13152,#13153,#13154,#13155,
#13156,#13157,#13158,#13159,#13160,#13161,#13162,#13163,#13164),
 .UNSPECIFIED.,.F.,.F.,(4,3,3,3,3,3,3,3,4),(0.,0.0238141989470671,0.0391004231578824,
0.0641320992313133,0.0780996136084711,0.101998806889826,0.113823260594808,
0.137564745199532,0.149565921982294),.UNSPECIFIED.);
#216=B_SPLINE_CURVE_WITH_KNOTS('',3,(#13166,#13167,#13168,#13169),
 .UNSPECIFIED.,.F.,.F.,(4,4),(2.76692059912875E-5,0.609394470571143),
 .UNSPECIFIED.);
#217=B_SPLINE_CURVE_WITH_KNOTS('',3,(#13172,#13173,#13174,#13175),
 .UNSPECIFIED.,.F.,.F.,(4,4),(0.809932799154201,3.21472245120952),
 .UNSPECIFIED.);
#218=B_SPLINE_CURVE_WITH_KNOTS('',3,(#13178,#13179,#13180,#13181,#13182,
#13183,#13184),.UNSPECIFIED.,.F.,.F.,(4,3,4),(3.41496637450242,5.11093193409745,
6.81591321610411),.UNSPECIFIED.);
#219=B_SPLINE_CURVE_WITH_KNOTS('',3,(#13188,#13189,#13190,#13191),
 .UNSPECIFIED.,.F.,.F.,(4,4),(9.91798263530139,10.2237206759544),
 .UNSPECIFIED.);
#220=B_SPLINE_CURVE_WITH_KNOTS('',3,(#13193,#13194,#13195,#13196,#13197,
#13198,#13199,#13200,#13201,#13202,#13203,#13204,#13205,#13206,#13207,#13208,
#13209,#13210,#13211,#13212,#13213,#13214,#13215,#13216,#13217,#13218,#13219,
#13220),.UNSPECIFIED.,.F.,.F.,(4,3,3,3,3,3,3,3,3,4),(0.,0.023807020713713,
0.039085080816122,0.0628703378723092,0.0651394887354207,0.0780750047750988,
0.101981498769656,0.114997221725907,0.138748569029605,0.151942344104828),
 .UNSPECIFIED.);
#221=B_SPLINE_CURVE_WITH_KNOTS('',3,(#13224,#13225,#13226,#13227,#13228,
#13229,#13230,#13231,#13232,#13233,#13234,#13235,#13236,#13237,#13238,#13239,
#13240,#13241,#13242,#13243,#13244,#13245,#13246,#13247,#13248,#13249,#13250,
#13251),.UNSPECIFIED.,.F.,.F.,(4,3,3,3,3,3,3,3,3,4),(0.,0.0238098191818892,
0.0391006681981376,0.0628849269680955,0.0651459659463291,0.0780999162396042,
0.102007524384594,0.115011225379555,0.138759376430353,0.151943200125079),
 .UNSPECIFIED.);
#222=B_SPLINE_CURVE_WITH_KNOTS('',3,(#13253,#13254,#13255,#13256),
 .UNSPECIFIED.,.F.,.F.,(4,4),(2.85486020485948E-5,0.305707210239178),
 .UNSPECIFIED.);
#223=B_SPLINE_CURVE_WITH_KNOTS('',3,(#13266,#13267,#13268,#13269,#13270,
#13271),.UNSPECIFIED.,.F.,.F.,(4,2,4),(-0.606446248197249,-0.303383959626182,
-6.4365448350312E-5),.UNSPECIFIED.);
#224=B_SPLINE_CURVE_WITH_KNOTS('',3,(#13273,#13274,#13275,#13276,#13277,
#13278),.UNSPECIFIED.,.F.,.F.,(4,2,4),(-0.60675170080159,-0.303384112192838,
-0.000369837888147484),.UNSPECIFIED.);
#225=B_SPLINE_CURVE_WITH_KNOTS('',3,(#13280,#13281,#13282,#13283,#13284,
#13285,#13286,#13287,#13288,#13289,#13290,#13291,#13292,#13293,#13294,#13295,
#13296,#13297,#13298,#13299,#13300,#13301,#13302,#13303,#13304,#13305,#13306,
#13307),.UNSPECIFIED.,.F.,.F.,(4,3,3,3,3,3,3,3,3,4),(-0.152162866344201,
-0.128411131698784,-0.115108013904405,-0.0911850729173883,-0.0780642464630149,
-0.0652023242402653,-0.0414053499882389,-0.0390151293250392,-0.0152279490549848,
0.),.UNSPECIFIED.);
#226=B_SPLINE_CURVE_WITH_KNOTS('',3,(#13310,#13311,#13312,#13313,#13314,
#13315,#13316,#13317,#13318,#13319,#13320,#13321,#13322,#13323,#13324,#13325,
#13326,#13327,#13328,#13329,#13330,#13331,#13332,#13333,#13334,#13335,#13336,
#13337),.UNSPECIFIED.,.F.,.F.,(4,3,3,3,3,3,3,3,3,4),(-0.152171297476962,
-0.128400300768352,-0.115247520946962,-0.0914735511738372,-0.0869860114952295,
-0.0783112904282795,-0.0544025203706761,-0.0391699941254272,-0.015391764586027,
0.),.UNSPECIFIED.);
#227=B_SPLINE_CURVE_WITH_KNOTS('',3,(#13354,#13355,#13356,#13357),
 .UNSPECIFIED.,.F.,.F.,(4,4),(-3.45733745322815,-0.757207059295936),
 .UNSPECIFIED.);
#228=B_SPLINE_CURVE_WITH_KNOTS('',3,(#13375,#13376,#13377,#13378),
 .UNSPECIFIED.,.F.,.F.,(4,4),(-0.557056952888827,-0.283259008618247),
 .UNSPECIFIED.);
#229=B_SPLINE_CURVE_WITH_KNOTS('',3,(#13379,#13380,#13381,#13382),
 .UNSPECIFIED.,.F.,.F.,(4,4),(-0.618164468641375,-0.0110156167597059),
 .UNSPECIFIED.);
#230=B_SPLINE_CURVE_WITH_KNOTS('',3,(#13424,#13425,#13426,#13427),
 .UNSPECIFIED.,.F.,.F.,(4,4),(0.283259011433088,0.551788488929761),
 .UNSPECIFIED.);
#231=B_SPLINE_CURVE_WITH_KNOTS('',3,(#13431,#13432,#13433,#13434),
 .UNSPECIFIED.,.F.,.F.,(4,4),(10.1507419987596,10.419271481025),
 .UNSPECIFIED.);
#232=B_SPLINE_CURVE_WITH_KNOTS('',3,(#13469,#13470,#13471,#13472),
 .UNSPECIFIED.,.F.,.F.,(4,4),(0.0110156167597055,0.618164468641375),
 .UNSPECIFIED.);
#233=B_SPLINE_CURVE_WITH_KNOTS('',3,(#13473,#13474,#13475,#13476),
 .UNSPECIFIED.,.F.,.F.,(4,4),(-10.419271481025,-10.1454735367545),
 .UNSPECIFIED.);
#234=B_SPLINE_CURVE_WITH_KNOTS('',3,(#13479,#13480,#13481,#13482,#13483,
#13484),.UNSPECIFIED.,.F.,.F.,(4,2,4),(-0.606211482799139,-0.303431960476852,
-9.19895310989571E-5),.UNSPECIFIED.);
#235=B_SPLINE_CURVE_WITH_KNOTS('',3,(#13486,#13487,#13488,#13489,#13490,
#13491,#13492,#13493,#13494,#13495,#13496,#13497,#13498,#13499,#13500,#13501,
#13502,#13503,#13504,#13505,#13506,#13507,#13508,#13509,#13510,#13511,#13512,
#13513),.UNSPECIFIED.,.F.,.F.,(4,3,3,3,3,3,3,3,3,4),(-0.152283340966725,
-0.128554242174982,-0.115196092098682,-0.0912819860997417,-0.0781117853096875,
-0.0652755629514801,-0.0414857317972147,-0.039051434275634,-0.0152612146291672,
0.),.UNSPECIFIED.);
#236=B_SPLINE_CURVE_WITH_KNOTS('',3,(#13517,#13518,#13519,#13520,#13521,
#13522,#13523,#13524,#13525,#13526,#13527,#13528,#13529,#13530,#13531,#13532,
#13533,#13534,#13535,#13536,#13537,#13538,#13539,#13540,#13541,#13542,#13543,
#13544),.UNSPECIFIED.,.F.,.F.,(4,3,3,3,3,3,3,3,3,4),(-0.152285570909379,
-0.128511627155755,-0.115232904621082,-0.0914664612111958,-0.0870286654075453,
-0.0781769338106538,-0.0542752301960614,-0.039092246575741,-0.0153386136911565,
0.),.UNSPECIFIED.);
#237=B_SPLINE_CURVE_WITH_KNOTS('',3,(#13545,#13546,#13547,#13548,#13549,
#13550),.UNSPECIFIED.,.F.,.F.,(4,2,4),(-0.606773318344362,-0.303431998667662,
-0.000653802131222458),.UNSPECIFIED.);
#238=B_SPLINE_CURVE_WITH_KNOTS('',3,(#13567,#13568,#13569,#13570),
 .UNSPECIFIED.,.F.,.F.,(4,4),(-7.05313168653828,-3.6572084986735),
 .UNSPECIFIED.);
#239=B_SPLINE_CURVE_WITH_KNOTS('',3,(#13591,#13592,#13593,#13594),
 .UNSPECIFIED.,.F.,.F.,(4,4),(3.65450559744172,7.0548588409572),
 .UNSPECIFIED.);
#240=B_SPLINE_CURVE_WITH_KNOTS('',3,(#13596,#13597,#13598,#13599),
 .UNSPECIFIED.,.F.,.F.,(4,4),(3.64767164868607,7.04802489220155),
 .UNSPECIFIED.);
#241=B_SPLINE_CURVE_WITH_KNOTS('',3,(#13620,#13621,#13622,#13623),
 .UNSPECIFIED.,.F.,.F.,(4,4),(-7.04532199096977,-3.64939880310499),
 .UNSPECIFIED.);
#242=B_SPLINE_CURVE_WITH_KNOTS('',3,(#13642,#13643,#13644,#13645,#13646,
#13647),.UNSPECIFIED.,.F.,.F.,(4,2,4),(-0.606200453641641,-0.30343602424441,
-9.0120313562092E-5),.UNSPECIFIED.);
#243=B_SPLINE_CURVE_WITH_KNOTS('',3,(#13649,#13650,#13651,#13652,#13653,
#13654,#13655,#13656,#13657,#13658,#13659,#13660,#13661,#13662,#13663,#13664,
#13665,#13666,#13667,#13668,#13669,#13670,#13671,#13672,#13673,#13674,#13675,
#13676),.UNSPECIFIED.,.F.,.F.,(4,3,3,3,3,3,3,3,3,4),(-0.152277688086818,
-0.128551334178815,-0.115197577176818,-0.0912856014461669,-0.0781191417238373,
-0.0652765169533013,-0.0414883027365163,-0.0390570310290822,-0.0152653090895913,
0.),.UNSPECIFIED.);
#244=B_SPLINE_CURVE_WITH_KNOTS('',3,(#13678,#13679,#13680,#13681,#13682,
#13683),.UNSPECIFIED.,.F.,.F.,(4,2,4),(-0.60678286609787,-0.303436074842897,
-0.000672492961417026),.UNSPECIFIED.);
#245=B_SPLINE_CURVE_WITH_KNOTS('',3,(#13700,#13701,#13702,#13703),
 .UNSPECIFIED.,.F.,.F.,(4,4),(-9.65082888146972,-7.25285594219682),
 .UNSPECIFIED.);
#246=B_SPLINE_CURVE_WITH_KNOTS('',3,(#13724,#13725,#13726,#13727),
 .UNSPECIFIED.,.F.,.F.,(4,4),(7.25489642332205,7.94751235889625),
 .UNSPECIFIED.);
#247=B_SPLINE_CURVE_WITH_KNOTS('',3,(#13728,#13729,#13730,#13731),
 .UNSPECIFIED.,.F.,.F.,(4,4),(8.17787511801303,9.65708648657758),
 .UNSPECIFIED.);
#248=B_SPLINE_CURVE_WITH_KNOTS('',3,(#13751,#13752,#13753,#13754,#13755,
#13756),.UNSPECIFIED.,.F.,.F.,(4,2,4),(-0.607007797795788,-0.303636495504298,
-0.000571323176327465),.UNSPECIFIED.);
#249=B_SPLINE_CURVE_WITH_KNOTS('',3,(#13758,#13759,#13760,#13761,#13762,
#13763,#13764,#13765,#13766,#13767,#13768,#13769,#13770,#13771,#13772,#13773,
#13774,#13775,#13776,#13777,#13778,#13779,#13780,#13781,#13782,#13783,#13784,
#13785),.UNSPECIFIED.,.F.,.F.,(4,3,3,3,3,3,3,3,3,4),(-0.152184339020145,
-0.128410461444444,-0.115096394428865,-0.0911692948751363,-0.0780261759644403,
-0.0651939085034322,-0.0413932235702045,-0.0389860720679279,-0.0151971168406065,
0.),.UNSPECIFIED.);
#250=B_SPLINE_CURVE_WITH_KNOTS('',3,(#13789,#13790,#13791,#13792,#13793,
#13794,#13795,#13796,#13797,#13798,#13799,#13800,#13801,#13802,#13803,#13804,
#13805,#13806,#13807,#13808,#13809,#13810,#13811,#13812,#13813,#13814,#13815,
#13816),.UNSPECIFIED.,.F.,.F.,(4,3,3,3,3,3,3,3,3,4),(-0.15219777746951,
-0.128424216118147,-0.115318679085322,-0.0915406112613293,-0.0870190514838729,
-0.0784197287877601,-0.0545085386658457,-0.0392329067084975,-0.0154317870320417,
0.),.UNSPECIFIED.);
#251=B_SPLINE_CURVE_WITH_KNOTS('',3,(#13817,#13818,#13819,#13820,#13821,
#13822),.UNSPECIFIED.,.F.,.F.,(4,2,4),(-0.606706256981509,-0.303636876939173,
-0.00026974181288697),.UNSPECIFIED.);
#252=B_SPLINE_CURVE_WITH_KNOTS('',3,(#13840,#13841,#13842,#13843),
 .UNSPECIFIED.,.F.,.F.,(4,4),(0.0112334529114386,0.618489359031386),
 .UNSPECIFIED.);
#253=B_SPLINE_CURVE_WITH_KNOTS('',3,(#13844,#13845,#13846,#13847),
 .UNSPECIFIED.,.F.,.F.,(4,4),(-10.4271318523291,-9.85085636625011),
 .UNSPECIFIED.);
#254=B_SPLINE_CURVE_WITH_KNOTS('',3,(#13870,#13871,#13872,#13873),
 .UNSPECIFIED.,.F.,.F.,(4,4),(9.85750350611301,10.4271318523291),
 .UNSPECIFIED.);
#255=B_SPLINE_CURVE_WITH_KNOTS('',3,(#13877,#13878,#13879,#13880),
 .UNSPECIFIED.,.F.,.F.,(4,4),(0.27539863731415,0.845026983530265),
 .UNSPECIFIED.);
#256=B_SPLINE_CURVE_WITH_KNOTS('',3,(#13898,#13899,#13900,#13901),
 .UNSPECIFIED.,.F.,.F.,(4,4),(-0.851674123393175,-0.27539863731415),
 .UNSPECIFIED.);
#257=B_SPLINE_CURVE_WITH_KNOTS('',3,(#13902,#13903,#13904,#13905),
 .UNSPECIFIED.,.F.,.F.,(4,4),(-0.618489359031386,-0.0112334529114389),
 .UNSPECIFIED.);
#258=B_SPLINE_CURVE_WITH_KNOTS('',3,(#13985,#13986,#13987,#13988),
 .UNSPECIFIED.,.F.,.F.,(4,4),(0.0112755522169305,0.618164468641375),
 .UNSPECIFIED.);
#259=B_SPLINE_CURVE_WITH_KNOTS('',3,(#14009,#14010,#14011,#14012),
 .UNSPECIFIED.,.F.,.F.,(4,4),(-0.618164468641375,-0.0112755522169305),
 .UNSPECIFIED.);
#260=B_SPLINE_CURVE_WITH_KNOTS('',3,(#14098,#14099,#14100,#14101),
 .UNSPECIFIED.,.F.,.F.,(4,4),(5.55111512312578E-17,0.618489359031386),
 .UNSPECIFIED.);
#261=B_SPLINE_CURVE_WITH_KNOTS('',3,(#14102,#14103,#14104,#14105),
 .UNSPECIFIED.,.F.,.F.,(4,4),(-0.618489359031386,-0.00110654915602034),
 .UNSPECIFIED.);
#262=B_SPLINE_CURVE_WITH_KNOTS('',3,(#14141,#14142,#14143,#14144,#14145),
 .UNSPECIFIED.,.F.,.F.,(4,1,4),(-10.4271318523291,-4.63063308449434,-0.283259008618247),
 .UNSPECIFIED.);
#263=B_SPLINE_CURVE_WITH_KNOTS('',3,(#14146,#14147,#14148,#14149,#14150),
 .UNSPECIFIED.,.F.,.F.,(4,1,4),(0.283259011433087,4.63063308449434,10.4271318523291),
 .UNSPECIFIED.);
#264=B_SPLINE_CURVE_WITH_KNOTS('',3,(#14171,#14172,#14173,#14174),
 .UNSPECIFIED.,.F.,.F.,(4,4),(0.000779732613545348,0.618164468641375),
 .UNSPECIFIED.);
#265=B_SPLINE_CURVE_WITH_KNOTS('',3,(#14175,#14176,#14177,#14178),
 .UNSPECIFIED.,.F.,.F.,(4,4),(-0.618164468641375,-4.9439619065339E-17),
 .UNSPECIFIED.);
#266=B_SPLINE_CURVE_WITH_KNOTS('',3,(#14199,#14200,#14201,#14202),
 .UNSPECIFIED.,.F.,.F.,(4,4),(3.0964814046186E-16,0.618164468641375),
 .UNSPECIFIED.);
#267=B_SPLINE_CURVE_WITH_KNOTS('',3,(#14203,#14204,#14205,#14206),
 .UNSPECIFIED.,.F.,.F.,(4,4),(-0.618164468641375,-0.0007797326135453),
 .UNSPECIFIED.);
#268=B_SPLINE_CURVE_WITH_KNOTS('',3,(#14232,#14233,#14234,#14235,#14236),
 .UNSPECIFIED.,.F.,.F.,(4,1,4),(-10.419271481025,-4.62277271319024,-0.27539863731415),
 .UNSPECIFIED.);
#269=B_SPLINE_CURVE_WITH_KNOTS('',3,(#14237,#14238,#14239,#14240,#14241),
 .UNSPECIFIED.,.F.,.F.,(4,1,4),(0.27539863731415,4.62277271319024,10.419271481025),
 .UNSPECIFIED.);
#270=B_SPLINE_CURVE_WITH_KNOTS('',3,(#14262,#14263,#14264,#14265),
 .UNSPECIFIED.,.F.,.F.,(4,4),(0.00110654915602046,0.618489359031386),
 .UNSPECIFIED.);
#271=B_SPLINE_CURVE_WITH_KNOTS('',3,(#14266,#14267,#14268,#14269),
 .UNSPECIFIED.,.F.,.F.,(4,4),(-0.618489359031386,6.93889390390723E-18),
 .UNSPECIFIED.);
#272=B_SPLINE_CURVE_WITH_KNOTS('',3,(#14309,#14310,#14311,#14312,#14313,
#14314,#14315,#14316,#14317,#14318,#14319,#14320,#14321,#14322,#14323,#14324,
#14325,#14326,#14327,#14328,#14329,#14330,#14331,#14332),.UNSPECIFIED.,
 .F.,.F.,(4,2,2,2,2,2,2,2,2,2,2,4),(-0.337265338267783,-0.250544943628509,
-0.208272806508042,-0.186542211788094,-0.176382978682897,-0.170925844043069,
-0.16639450677335,-0.161077381235501,-0.15182241135393,-0.115009181549223,
-0.030206004227969,0.),.UNSPECIFIED.);
#273=B_SPLINE_CURVE_WITH_KNOTS('',3,(#14337,#14338,#14339,#14340,#14341,
#14342,#14343,#14344,#14345,#14346,#14347,#14348,#14349,#14350,#14351,#14352,
#14353,#14354,#14355,#14356),.UNSPECIFIED.,.F.,.F.,(4,2,2,2,2,2,2,2,2,4),
(-0.240982594686416,-0.16829976149504,-0.141836598208813,-0.129116059226128,
-0.121962912034391,-0.115857591426886,-0.108506552485159,-0.0948769875819265,
-0.0364654790774683,0.),.UNSPECIFIED.);
#274=B_SPLINE_CURVE_WITH_KNOTS('',3,(#14361,#14362,#14363,#14364,#14365,
#14366,#14367,#14368,#14369,#14370,#14371,#14372,#14373,#14374,#14375,#14376,
#14377,#14378,#14379,#14380),.UNSPECIFIED.,.F.,.F.,(4,2,2,2,2,2,2,2,2,4),
(-0.240981214998207,-0.168303541671295,-0.141841407502325,-0.129121097580905,
-0.121968013294536,-0.115862708924237,-0.108511643765797,-0.0948818976588229,
-0.0364681276985956,0.),.UNSPECIFIED.);
#275=B_SPLINE_CURVE_WITH_KNOTS('',3,(#14385,#14386,#14387,#14388,#14389,
#14390,#14391,#14392,#14393,#14394,#14395,#14396,#14397,#14398,#14399,#14400,
#14401,#14402,#14403,#14404,#14405,#14406,#14407,#14408),.UNSPECIFIED.,
 .F.,.F.,(4,2,2,2,2,2,2,2,2,2,2,4),(-0.337269388373684,-0.250545316912909,
-0.208282401844766,-0.186554569827561,-0.176396213396297,-0.17093921790305,
-0.16640782243471,-0.161090427650893,-0.151834477986603,-0.115010808423941,
-0.0302102096065556,0.),.UNSPECIFIED.);
#276=B_SPLINE_CURVE_WITH_KNOTS('',3,(#14431,#14432,#14433,#14434),
 .UNSPECIFIED.,.F.,.F.,(4,4),(1.0454440030657,2.52465537163019),
 .UNSPECIFIED.);
#277=B_SPLINE_CURVE_WITH_KNOTS('',3,(#14436,#14437,#14438,#14439,#14440,
#14441,#14442,#14443,#14444,#14445,#14446,#14447,#14448,#14449,#14450,#14451,
#14452,#14453,#14454,#14455,#14456,#14457,#14458,#14459,#14460,#14461,#14462,
#14463),.UNSPECIFIED.,.F.,.F.,(4,3,3,3,3,3,3,3,3,4),(-0.152193408756968,
-0.128427023368412,-0.115107736263918,-0.0911810900745799,-0.0780377802127556,
-0.0652031397886901,-0.0414031558437525,-0.0389949527774582,-0.0152076153333754,
0.),.UNSPECIFIED.);
#278=B_SPLINE_CURVE_WITH_KNOTS('',3,(#14465,#14466,#14467,#14468),
 .UNSPECIFIED.,.F.,.F.,(4,4),(-3.44967454744645,-1.05170160817356),
 .UNSPECIFIED.);
#279=B_SPLINE_CURVE_WITH_KNOTS('',3,(#14470,#14471,#14472,#14473,#14474,
#14475,#14476,#14477,#14478,#14479,#14480,#14481,#14482,#14483,#14484,#14485,
#14486,#14487,#14488,#14489,#14490,#14491,#14492,#14493,#14494,#14495,#14496,
#14497),.UNSPECIFIED.,.F.,.F.,(4,3,3,3,3,3,3,3,3,4),(-0.152278960443096,
-0.128503570101575,-0.115218572146868,-0.09145408274965,-0.0870214650669139,
-0.0781562978024333,-0.0542566895399357,-0.03908030849237,-0.0153296112319379,
0.),.UNSPECIFIED.);
#280=B_SPLINE_CURVE_WITH_KNOTS('',3,(#14498,#14499,#14500,#14501),
 .UNSPECIFIED.,.F.,.F.,(4,4),(2.75501813708031,3.4476340663212),
 .UNSPECIFIED.);
#281=B_SPLINE_CURVE_WITH_KNOTS('',3,(#14523,#14524,#14525,#14526),
 .UNSPECIFIED.,.F.,.F.,(4,4),(7.24810383506675,7.89761558728778),
 .UNSPECIFIED.);
#282=B_SPLINE_CURVE_WITH_KNOTS('',3,(#14528,#14529,#14530,#14531,#14532,
#14533,#14534,#14535,#14536,#14537,#14538,#14539,#14540,#14541,#14542,#14543,
#14544,#14545,#14546,#14547,#14548,#14549,#14550,#14551,#14552,#14553,#14554,
#14555),.UNSPECIFIED.,.F.,.F.,(4,3,3,3,3,3,3,3,3,4),(-0.152278869104567,
-0.128548794904564,-0.115192257893812,-0.0912773536606376,-0.0781090575823055,
-0.0652724057916263,-0.0414819581560496,-0.0390493575290778,-0.015259721743698,
0.),.UNSPECIFIED.);
#283=B_SPLINE_CURVE_WITH_KNOTS('',3,(#14557,#14558,#14559,#14560),
 .UNSPECIFIED.,.F.,.F.,(4,4),(-9.94532343034734,-7.24519303641511),
 .UNSPECIFIED.);
#284=B_SPLINE_CURVE_WITH_KNOTS('',3,(#14562,#14563,#14564,#14565,#14566,
#14567,#14568,#14569,#14570,#14571,#14572,#14573,#14574,#14575,#14576,#14577,
#14578,#14579,#14580,#14581,#14582,#14583,#14584,#14585,#14586,#14587,#14588,
#14589),.UNSPECIFIED.,.F.,.F.,(4,3,3,3,3,3,3,3,3,4),(-0.152181623618259,
-0.128410404494075,-0.115248188224843,-0.0914746846046984,-0.0869904866333268,
-0.0783028696190655,-0.0543945376065823,-0.0391651209697638,-0.0153884182770307,
0.),.UNSPECIFIED.);
#285=B_SPLINE_CURVE_WITH_KNOTS('',3,(#14590,#14591,#14592,#14593),
 .UNSPECIFIED.,.F.,.F.,(4,4),(8.21380824320284,9.95046871680089),
 .UNSPECIFIED.);
#286=B_SPLINE_CURVE_WITH_KNOTS('',3,(#14596,#14597,#14598,#14599),
 .UNSPECIFIED.,.F.,.F.,(4,4),(2.80491490332713,3.45442665446657),
 .UNSPECIFIED.);
#287=B_SPLINE_CURVE_WITH_KNOTS('',3,(#14603,#14604,#14605,#14606),
 .UNSPECIFIED.,.F.,.F.,(4,4),(0.752061768057538,2.48872224644044),
 .UNSPECIFIED.);
#288=B_SPLINE_CURVE_WITH_KNOTS('',3,(#14814,#14815,#14816,#14817,#14818,
#14819),.UNSPECIFIED.,.F.,.F.,(4,2,4),(-0.606700505977711,-0.303383635264422,
-0.000339350725729326),.UNSPECIFIED.);
#289=B_SPLINE_CURVE_WITH_KNOTS('',3,(#14820,#14821,#14822,#14823,#14824,
#14825,#14826,#14827,#14828,#14829,#14830,#14831,#14832,#14833,#14834,#14835,
#14836,#14837,#14838,#14839,#14840,#14841,#14842,#14843,#14844,#14845,#14846,
#14847),.UNSPECIFIED.,.F.,.F.,(4,3,3,3,3,3,3,3,3,4),(-0.152173579228948,
-0.128423230539522,-0.115115104157663,-0.0911927259648815,-0.0780672068328041,
-0.0652082609452843,-0.0414117413801899,-0.0390174000215468,-0.0152300060615686,
0.),.UNSPECIFIED.);
#290=B_SPLINE_CURVE_WITH_KNOTS('',3,(#14848,#14849,#14850,#14851,#14852,
#14853),.UNSPECIFIED.,.F.,.F.,(4,2,4),(-0.606471894652381,-0.303383500305553,
-0.00011071898471493),.UNSPECIFIED.);
#291=B_SPLINE_CURVE_WITH_KNOTS('',3,(#14857,#14858,#14859,#14860,#14861,
#14862),.UNSPECIFIED.,.F.,.F.,(4,2,4),(-0.606240625011114,-0.303433113375332,
-0.00010938105916114),.UNSPECIFIED.);
#292=B_SPLINE_CURVE_WITH_KNOTS('',3,(#14864,#14865,#14866,#14867,#14868,
#14869,#14870,#14871,#14872,#14873,#14874,#14875,#14876,#14877,#14878,#14879,
#14880,#14881,#14882,#14883,#14884,#14885,#14886,#14887,#14888,#14889,#14890,
#14891),.UNSPECIFIED.,.F.,.F.,(4,3,3,3,3,3,3,3,3,4),(-0.152281454644235,
-0.128508102092242,-0.115234945630277,-0.0914677943501604,-0.0870276017853555,
-0.0781846052914712,-0.0542821334115454,-0.0390966859411886,-0.0153419673568312,
0.),.UNSPECIFIED.);
#293=B_SPLINE_CURVE_WITH_KNOTS('',3,(#14893,#14894,#14895,#14896,#14897,
#14898),.UNSPECIFIED.,.F.,.F.,(4,2,4),(-0.606758573154242,-0.303433157101101,
-0.000627306481538803),.UNSPECIFIED.);
#294=B_SPLINE_CURVE_WITH_KNOTS('',3,(#14904,#14905,#14906,#14907,#14908,
#14909),.UNSPECIFIED.,.F.,.F.,(4,2,4),(-0.60617382748,-0.303436117212405,
-7.2700296824213E-5),.UNSPECIFIED.);
#295=B_SPLINE_CURVE_WITH_KNOTS('',3,(#14911,#14912,#14913,#14914,#14915,
#14916,#14917,#14918,#14919,#14920,#14921,#14922,#14923,#14924,#14925,#14926,
#14927,#14928,#14929,#14930,#14931,#14932,#14933,#14934,#14935,#14936,#14937,
#14938),.UNSPECIFIED.,.F.,.F.,(4,3,3,3,3,3,3,3,3,4),(-0.152282154327755,
-0.128558036203745,-0.115201429639692,-0.0912891813973639,-0.0781219052297615,
-0.065279687589213,-0.0414913146723999,-0.0390591331507366,-0.0152683745546824,
0.),.UNSPECIFIED.);
#296=B_SPLINE_CURVE_WITH_KNOTS('',3,(#14942,#14943,#14944,#14945,#14946,
#14947,#14948,#14949,#14950,#14951,#14952,#14953,#14954,#14955,#14956,#14957,
#14958,#14959,#14960,#14961,#14962,#14963,#14964,#14965,#14966,#14967,#14968,
#14969),.UNSPECIFIED.,.F.,.F.,(4,3,3,3,3,3,3,3,3,4),(-0.152283066055976,
-0.128508717930245,-0.115216472798554,-0.091451700383826,-0.087022506454752,
-0.0781485278686168,-0.0542483994686567,-0.0390758108455304,-0.0153274175274101,
0.),.UNSPECIFIED.);
#297=B_SPLINE_CURVE_WITH_KNOTS('',3,(#14971,#14972,#14973,#14974,#14975,
#14976),.UNSPECIFIED.,.F.,.F.,(4,2,4),(-0.606800264911061,-0.303436147592132,
-0.000699137727853738),.UNSPECIFIED.);
#298=B_SPLINE_CURVE_WITH_KNOTS('',3,(#14981,#14982,#14983,#14984,#14985,
#14986),.UNSPECIFIED.,.F.,.F.,(4,2,4),(-0.606915279655722,-0.30363236403835,
-0.000516487074480598),.UNSPECIFIED.);
#299=B_SPLINE_CURVE_WITH_KNOTS('',3,(#14990,#14991,#14992,#14993,#14994,
#14995,#14996,#14997,#14998,#14999,#15000,#15001,#15002,#15003,#15004,#15005,
#15006,#15007,#15008,#15009,#15010,#15011,#15012,#15013,#15014,#15015,#15016,
#15017),.UNSPECIFIED.,.F.,.F.,(4,3,3,3,3,3,3,3,3,4),(-0.152205325335401,
-0.128433618138404,-0.115304790388008,-0.091527299141506,-0.0870178586418932,
-0.0783866443643876,-0.0544751548276533,-0.0392137310602028,-0.0154203878854647,
0.),.UNSPECIFIED.);
#300=B_SPLINE_CURVE_WITH_KNOTS('',3,(#15019,#15020,#15021,#15022,#15023,
#15024),.UNSPECIFIED.,.F.,.F.,(4,2,4),(-0.606752424187958,-0.303632696349781,
-0.000353591088346872),.UNSPECIFIED.);
#301=B_SPLINE_CURVE_WITH_KNOTS('',3,(#15030,#15031,#15032,#15033),
 .UNSPECIFIED.,.F.,.F.,(4,4),(0.0116023361771303,0.618489359031386),
 .UNSPECIFIED.);
#302=B_SPLINE_CURVE_WITH_KNOTS('',3,(#15037,#15038,#15039,#15040),
 .UNSPECIFIED.,.F.,.F.,(4,4),(-0.618489359031386,-0.01160233617713),
 .UNSPECIFIED.);
#303=B_SPLINE_CURVE_WITH_KNOTS('',3,(#15043,#15044,#15045,#15046),
 .UNSPECIFIED.,.F.,.F.,(4,4),(7.01593971618694,9.71770560667459),
 .UNSPECIFIED.);
#304=B_SPLINE_CURVE_WITH_KNOTS('',3,(#15047,#15048,#15049,#15050),
 .UNSPECIFIED.,.F.,.F.,(4,4),(0.505945342046796,3.20718651982575),
 .UNSPECIFIED.);
#305=B_SPLINE_CURVE_WITH_KNOTS('',3,(#15053,#15054,#15055,#15056,#15057,
#15058,#15059),.UNSPECIFIED.,.F.,.F.,(4,3,4),(3.40717417387402,5.11170895874517,
6.80746068626633),.UNSPECIFIED.);
#306=B_SPLINE_CURVE_WITH_KNOTS('',3,(#15062,#15063,#15064,#15065),
 .UNSPECIFIED.,.F.,.F.,(4,4),(7.00766573366377,9.41198845520559),
 .UNSPECIFIED.);
#307=B_SPLINE_CURVE_WITH_KNOTS('',3,(#15069,#15070,#15071,#15072),
 .UNSPECIFIED.,.F.,.F.,(4,4),(9.61248784142317,10.2217363065808),
 .UNSPECIFIED.);
#308=B_SPLINE_CURVE_WITH_KNOTS('',3,(#15073,#15074,#15075,#15076,#15077,
#15078,#15079,#15080,#15081,#15082,#15083,#15084,#15085,#15086,#15087,#15088,
#15089,#15090,#15091,#15092,#15093,#15094,#15095,#15096,#15097,#15098,#15099,
#15100),.UNSPECIFIED.,.F.,.F.,(4,3,3,3,3,3,3,3,3,4),(0.,0.0238103109064959,
0.0390781362249314,0.0628635086275546,0.0641230352384255,0.0780643700703951,
0.101962174814111,0.113803522271848,0.137549611554782,0.149564734365165),
 .UNSPECIFIED.);
#309=B_SPLINE_CURVE_WITH_KNOTS('',3,(#15104,#15105,#15106,#15107,#15108,
#15109,#15110,#15111,#15112,#15113,#15114,#15115,#15116,#15117,#15118,#15119,
#15120,#15121,#15122,#15123,#15124,#15125,#15126,#15127,#15128,#15129,#15130,
#15131,#15132,#15133,#15134),.UNSPECIFIED.,.F.,.F.,(4,3,3,3,3,3,3,3,3,3,
4),(0.,0.0535521515156599,0.107729685495911,0.117233338918226,0.171447998942947,
0.1923696899792,0.234191611538245,0.288659693466396,0.341410301570312,0.395549383747909,
0.448696573746633),.UNSPECIFIED.);
#310=B_SPLINE_CURVE_WITH_KNOTS('',3,(#15136,#15137,#15138,#15139),
 .UNSPECIFIED.,.F.,.F.,(4,4),(0.0255858263485814,0.973760737485873),
 .UNSPECIFIED.);
#311=B_SPLINE_CURVE_WITH_KNOTS('',3,(#15141,#15142,#15143,#15144,#15145,
#15146,#15147,#15148,#15149,#15150,#15151,#15152,#15153,#15154,#15155,#15156,
#15157,#15158,#15159,#15160,#15161,#15162,#15163,#15164,#15165,#15166,#15167,
#15168,#15169,#15170,#15171),.UNSPECIFIED.,.F.,.F.,(4,3,3,3,3,3,3,3,3,3,
4),(0.,0.0535144560117858,0.107726856902975,0.117300577410231,0.171517675930231,
0.195438847090422,0.234297456941738,0.289665153342662,0.345032849743585,
0.40043206955427,0.455831289364955),.UNSPECIFIED.);
#312=B_SPLINE_CURVE_WITH_KNOTS('',3,(#15175,#15176,#15177,#15178,#15179,
#15180,#15181,#15182,#15183,#15184,#15185,#15186,#15187,#15188,#15189,#15190,
#15191,#15192,#15193,#15194,#15195,#15196,#15197,#15198,#15199,#15200,#15201,
#15202,#15203,#15204,#15205),.UNSPECIFIED.,.F.,.F.,(4,3,3,3,3,3,3,3,3,3,
4),(0.,0.053505543180391,0.107714168832353,0.117253997025819,0.171473395203321,
0.195418854185489,0.234223199196375,0.289607016015183,0.344990832833991,
0.400409777473312,0.455828722112633),.UNSPECIFIED.);
#313=B_SPLINE_CURVE_WITH_KNOTS('',3,(#15207,#15208,#15209,#15210),
 .UNSPECIFIED.,.F.,.F.,(4,4),(0.0262392625141271,0.974414173651419),
 .UNSPECIFIED.);
#314=B_SPLINE_CURVE_WITH_KNOTS('',3,(#15212,#15213,#15214,#15215,#15216,
#15217,#15218,#15219,#15220,#15221,#15222,#15223,#15224,#15225,#15226,#15227,
#15228,#15229,#15230,#15231,#15232,#15233,#15234,#15235,#15236,#15237,#15238,
#15239,#15240,#15241,#15242),.UNSPECIFIED.,.F.,.F.,(4,3,3,3,3,3,3,3,3,3,
4),(0.,0.0535648734523888,0.107747221190676,0.117299947751206,0.171510987106922,
0.192397607227928,0.234296687348373,0.288768001369001,0.341469499352622,
0.395597672314973,0.448700135162036),.UNSPECIFIED.);
#315=B_SPLINE_CURVE_WITH_KNOTS('',3,(#15245,#15246,#15247,#15248,#15249,
#15250,#15251,#15252,#15253,#15254,#15255,#15256,#15257,#15258,#15259,#15260,
#15261,#15262,#15263,#15264,#15265,#15266,#15267,#15268,#15269),
 .UNSPECIFIED.,.F.,.F.,(4,3,3,3,3,3,3,3,4),(0.,0.0238141989470671,0.0391004231578824,
0.0641320992313133,0.0780996136084711,0.101998806889826,0.113823260594808,
0.137564745199532,0.149565921982294),.UNSPECIFIED.);
#316=B_SPLINE_CURVE_WITH_KNOTS('',3,(#15271,#15272,#15273,#15274),
 .UNSPECIFIED.,.F.,.F.,(4,4),(2.76692059912875E-5,0.609394470571143),
 .UNSPECIFIED.);
#317=B_SPLINE_CURVE_WITH_KNOTS('',3,(#15277,#15278,#15279,#15280),
 .UNSPECIFIED.,.F.,.F.,(4,4),(0.809932799154201,3.21472245120952),
 .UNSPECIFIED.);
#318=B_SPLINE_CURVE_WITH_KNOTS('',3,(#15283,#15284,#15285,#15286,#15287,
#15288,#15289),.UNSPECIFIED.,.F.,.F.,(4,3,4),(3.41496637450242,5.11093193409745,
6.81591321610411),.UNSPECIFIED.);
#319=B_SPLINE_CURVE_WITH_KNOTS('',3,(#15293,#15294,#15295,#15296),
 .UNSPECIFIED.,.F.,.F.,(4,4),(9.91798263530139,10.2237206759544),
 .UNSPECIFIED.);
#320=B_SPLINE_CURVE_WITH_KNOTS('',3,(#15298,#15299,#15300,#15301,#15302,
#15303,#15304,#15305,#15306,#15307,#15308,#15309,#15310,#15311,#15312,#15313,
#15314,#15315,#15316,#15317,#15318,#15319,#15320,#15321,#15322,#15323,#15324,
#15325),.UNSPECIFIED.,.F.,.F.,(4,3,3,3,3,3,3,3,3,4),(0.,0.023807020713713,
0.039085080816122,0.0628703378723092,0.0651394887354207,0.0780750047750988,
0.101981498769656,0.114997221725907,0.138748569029605,0.151942344104828),
 .UNSPECIFIED.);
#321=B_SPLINE_CURVE_WITH_KNOTS('',3,(#15329,#15330,#15331,#15332,#15333,
#15334,#15335,#15336,#15337,#15338,#15339,#15340,#15341,#15342,#15343,#15344,
#15345,#15346,#15347,#15348,#15349,#15350,#15351,#15352,#15353,#15354,#15355,
#15356),.UNSPECIFIED.,.F.,.F.,(4,3,3,3,3,3,3,3,3,4),(0.,0.0238098191818892,
0.0391006681981376,0.0628849269680955,0.0651459659463291,0.0780999162396042,
0.102007524384594,0.115011225379555,0.138759376430353,0.151943200125079),
 .UNSPECIFIED.);
#322=B_SPLINE_CURVE_WITH_KNOTS('',3,(#15358,#15359,#15360,#15361),
 .UNSPECIFIED.,.F.,.F.,(4,4),(2.85486020485948E-5,0.305707210239178),
 .UNSPECIFIED.);
#323=B_SPLINE_CURVE_WITH_KNOTS('',3,(#15371,#15372,#15373,#15374,#15375,
#15376),.UNSPECIFIED.,.F.,.F.,(4,2,4),(-0.606446248197249,-0.303383959626182,
-6.4365448350312E-5),.UNSPECIFIED.);
#324=B_SPLINE_CURVE_WITH_KNOTS('',3,(#15378,#15379,#15380,#15381,#15382,
#15383),.UNSPECIFIED.,.F.,.F.,(4,2,4),(-0.60675170080159,-0.303384112192838,
-0.000369837888147484),.UNSPECIFIED.);
#325=B_SPLINE_CURVE_WITH_KNOTS('',3,(#15385,#15386,#15387,#15388,#15389,
#15390,#15391,#15392,#15393,#15394,#15395,#15396,#15397,#15398,#15399,#15400,
#15401,#15402,#15403,#15404,#15405,#15406,#15407,#15408,#15409,#15410,#15411,
#15412),.UNSPECIFIED.,.F.,.F.,(4,3,3,3,3,3,3,3,3,4),(-0.152162866344201,
-0.128411131698784,-0.115108013904405,-0.0911850729173883,-0.0780642464630149,
-0.0652023242402653,-0.0414053499882389,-0.0390151293250392,-0.0152279490549848,
0.),.UNSPECIFIED.);
#326=B_SPLINE_CURVE_WITH_KNOTS('',3,(#15415,#15416,#15417,#15418,#15419,
#15420,#15421,#15422,#15423,#15424,#15425,#15426,#15427,#15428,#15429,#15430,
#15431,#15432,#15433,#15434,#15435,#15436,#15437,#15438,#15439,#15440,#15441,
#15442),.UNSPECIFIED.,.F.,.F.,(4,3,3,3,3,3,3,3,3,4),(-0.152171297476962,
-0.128400300768352,-0.115247520946962,-0.0914735511738372,-0.0869860114952295,
-0.0783112904282795,-0.0544025203706761,-0.0391699941254272,-0.015391764586027,
0.),.UNSPECIFIED.);
#327=B_SPLINE_CURVE_WITH_KNOTS('',3,(#15459,#15460,#15461,#15462),
 .UNSPECIFIED.,.F.,.F.,(4,4),(-3.45733745322815,-0.757207059295936),
 .UNSPECIFIED.);
#328=B_SPLINE_CURVE_WITH_KNOTS('',3,(#15480,#15481,#15482,#15483),
 .UNSPECIFIED.,.F.,.F.,(4,4),(-0.557056952888827,-0.283259008618247),
 .UNSPECIFIED.);
#329=B_SPLINE_CURVE_WITH_KNOTS('',3,(#15484,#15485,#15486,#15487),
 .UNSPECIFIED.,.F.,.F.,(4,4),(-0.618164468641375,-0.0110156167597059),
 .UNSPECIFIED.);
#330=B_SPLINE_CURVE_WITH_KNOTS('',3,(#15529,#15530,#15531,#15532),
 .UNSPECIFIED.,.F.,.F.,(4,4),(0.283259011433088,0.551788488929761),
 .UNSPECIFIED.);
#331=B_SPLINE_CURVE_WITH_KNOTS('',3,(#15536,#15537,#15538,#15539),
 .UNSPECIFIED.,.F.,.F.,(4,4),(10.1507419987596,10.419271481025),
 .UNSPECIFIED.);
#332=B_SPLINE_CURVE_WITH_KNOTS('',3,(#15574,#15575,#15576,#15577),
 .UNSPECIFIED.,.F.,.F.,(4,4),(0.0110156167597055,0.618164468641375),
 .UNSPECIFIED.);
#333=B_SPLINE_CURVE_WITH_KNOTS('',3,(#15578,#15579,#15580,#15581),
 .UNSPECIFIED.,.F.,.F.,(4,4),(-10.419271481025,-10.1454735367545),
 .UNSPECIFIED.);
#334=B_SPLINE_CURVE_WITH_KNOTS('',3,(#15584,#15585,#15586,#15587,#15588,
#15589),.UNSPECIFIED.,.F.,.F.,(4,2,4),(-0.606211482799139,-0.303431960476852,
-9.19895310989571E-5),.UNSPECIFIED.);
#335=B_SPLINE_CURVE_WITH_KNOTS('',3,(#15591,#15592,#15593,#15594,#15595,
#15596,#15597,#15598,#15599,#15600,#15601,#15602,#15603,#15604,#15605,#15606,
#15607,#15608,#15609,#15610,#15611,#15612,#15613,#15614,#15615,#15616,#15617,
#15618),.UNSPECIFIED.,.F.,.F.,(4,3,3,3,3,3,3,3,3,4),(-0.152283340966725,
-0.128554242174982,-0.115196092098682,-0.0912819860997417,-0.0781117853096875,
-0.0652755629514801,-0.0414857317972147,-0.039051434275634,-0.0152612146291672,
0.),.UNSPECIFIED.);
#336=B_SPLINE_CURVE_WITH_KNOTS('',3,(#15622,#15623,#15624,#15625,#15626,
#15627,#15628,#15629,#15630,#15631,#15632,#15633,#15634,#15635,#15636,#15637,
#15638,#15639,#15640,#15641,#15642,#15643,#15644,#15645,#15646,#15647,#15648,
#15649),.UNSPECIFIED.,.F.,.F.,(4,3,3,3,3,3,3,3,3,4),(-0.152285570909379,
-0.128511627155755,-0.115232904621082,-0.0914664612111958,-0.0870286654075453,
-0.0781769338106538,-0.0542752301960614,-0.039092246575741,-0.0153386136911565,
0.),.UNSPECIFIED.);
#337=B_SPLINE_CURVE_WITH_KNOTS('',3,(#15650,#15651,#15652,#15653,#15654,
#15655),.UNSPECIFIED.,.F.,.F.,(4,2,4),(-0.606773318344362,-0.303431998667662,
-0.000653802131222458),.UNSPECIFIED.);
#338=B_SPLINE_CURVE_WITH_KNOTS('',3,(#15672,#15673,#15674,#15675),
 .UNSPECIFIED.,.F.,.F.,(4,4),(-7.05313168653828,-3.6572084986735),
 .UNSPECIFIED.);
#339=B_SPLINE_CURVE_WITH_KNOTS('',3,(#15696,#15697,#15698,#15699),
 .UNSPECIFIED.,.F.,.F.,(4,4),(3.65450559744172,7.0548588409572),
 .UNSPECIFIED.);
#340=B_SPLINE_CURVE_WITH_KNOTS('',3,(#15701,#15702,#15703,#15704),
 .UNSPECIFIED.,.F.,.F.,(4,4),(3.64767164868607,7.04802489220155),
 .UNSPECIFIED.);
#341=B_SPLINE_CURVE_WITH_KNOTS('',3,(#15725,#15726,#15727,#15728),
 .UNSPECIFIED.,.F.,.F.,(4,4),(-7.04532199096977,-3.64939880310499),
 .UNSPECIFIED.);
#342=B_SPLINE_CURVE_WITH_KNOTS('',3,(#15747,#15748,#15749,#15750,#15751,
#15752),.UNSPECIFIED.,.F.,.F.,(4,2,4),(-0.606200453641641,-0.30343602424441,
-9.0120313562092E-5),.UNSPECIFIED.);
#343=B_SPLINE_CURVE_WITH_KNOTS('',3,(#15754,#15755,#15756,#15757,#15758,
#15759,#15760,#15761,#15762,#15763,#15764,#15765,#15766,#15767,#15768,#15769,
#15770,#15771,#15772,#15773,#15774,#15775,#15776,#15777,#15778,#15779,#15780,
#15781),.UNSPECIFIED.,.F.,.F.,(4,3,3,3,3,3,3,3,3,4),(-0.152277688086818,
-0.128551334178815,-0.115197577176818,-0.0912856014461669,-0.0781191417238373,
-0.0652765169533013,-0.0414883027365163,-0.0390570310290822,-0.0152653090895913,
0.),.UNSPECIFIED.);
#344=B_SPLINE_CURVE_WITH_KNOTS('',3,(#15783,#15784,#15785,#15786,#15787,
#15788),.UNSPECIFIED.,.F.,.F.,(4,2,4),(-0.60678286609787,-0.303436074842897,
-0.000672492961417026),.UNSPECIFIED.);
#345=B_SPLINE_CURVE_WITH_KNOTS('',3,(#15805,#15806,#15807,#15808),
 .UNSPECIFIED.,.F.,.F.,(4,4),(-9.65082888146972,-7.25285594219682),
 .UNSPECIFIED.);
#346=B_SPLINE_CURVE_WITH_KNOTS('',3,(#15829,#15830,#15831,#15832),
 .UNSPECIFIED.,.F.,.F.,(4,4),(7.25489642332205,7.94751235889625),
 .UNSPECIFIED.);
#347=B_SPLINE_CURVE_WITH_KNOTS('',3,(#15833,#15834,#15835,#15836),
 .UNSPECIFIED.,.F.,.F.,(4,4),(8.17787511801303,9.65708648657758),
 .UNSPECIFIED.);
#348=B_SPLINE_CURVE_WITH_KNOTS('',3,(#15856,#15857,#15858,#15859,#15860,
#15861),.UNSPECIFIED.,.F.,.F.,(4,2,4),(-0.607007797795788,-0.303636495504298,
-0.000571323176327465),.UNSPECIFIED.);
#349=B_SPLINE_CURVE_WITH_KNOTS('',3,(#15863,#15864,#15865,#15866,#15867,
#15868,#15869,#15870,#15871,#15872,#15873,#15874,#15875,#15876,#15877,#15878,
#15879,#15880,#15881,#15882,#15883,#15884,#15885,#15886,#15887,#15888,#15889,
#15890),.UNSPECIFIED.,.F.,.F.,(4,3,3,3,3,3,3,3,3,4),(-0.152184339020145,
-0.128410461444444,-0.115096394428865,-0.0911692948751363,-0.0780261759644403,
-0.0651939085034322,-0.0413932235702045,-0.0389860720679279,-0.0151971168406065,
0.),.UNSPECIFIED.);
#350=B_SPLINE_CURVE_WITH_KNOTS('',3,(#15894,#15895,#15896,#15897,#15898,
#15899,#15900,#15901,#15902,#15903,#15904,#15905,#15906,#15907,#15908,#15909,
#15910,#15911,#15912,#15913,#15914,#15915,#15916,#15917,#15918,#15919,#15920,
#15921),.UNSPECIFIED.,.F.,.F.,(4,3,3,3,3,3,3,3,3,4),(-0.15219777746951,
-0.128424216118147,-0.115318679085322,-0.0915406112613293,-0.0870190514838729,
-0.0784197287877601,-0.0545085386658457,-0.0392329067084975,-0.0154317870320417,
0.),.UNSPECIFIED.);
#351=B_SPLINE_CURVE_WITH_KNOTS('',3,(#15922,#15923,#15924,#15925,#15926,
#15927),.UNSPECIFIED.,.F.,.F.,(4,2,4),(-0.606706256981509,-0.303636876939173,
-0.00026974181288697),.UNSPECIFIED.);
#352=B_SPLINE_CURVE_WITH_KNOTS('',3,(#15945,#15946,#15947,#15948),
 .UNSPECIFIED.,.F.,.F.,(4,4),(0.0112334529114386,0.618489359031386),
 .UNSPECIFIED.);
#353=B_SPLINE_CURVE_WITH_KNOTS('',3,(#15949,#15950,#15951,#15952),
 .UNSPECIFIED.,.F.,.F.,(4,4),(-10.4271318523291,-9.85085636625011),
 .UNSPECIFIED.);
#354=B_SPLINE_CURVE_WITH_KNOTS('',3,(#15975,#15976,#15977,#15978),
 .UNSPECIFIED.,.F.,.F.,(4,4),(9.85750350611301,10.4271318523291),
 .UNSPECIFIED.);
#355=B_SPLINE_CURVE_WITH_KNOTS('',3,(#15982,#15983,#15984,#15985),
 .UNSPECIFIED.,.F.,.F.,(4,4),(0.27539863731415,0.845026983530265),
 .UNSPECIFIED.);
#356=B_SPLINE_CURVE_WITH_KNOTS('',3,(#16003,#16004,#16005,#16006),
 .UNSPECIFIED.,.F.,.F.,(4,4),(-0.851674123393175,-0.27539863731415),
 .UNSPECIFIED.);
#357=B_SPLINE_CURVE_WITH_KNOTS('',3,(#16007,#16008,#16009,#16010),
 .UNSPECIFIED.,.F.,.F.,(4,4),(-0.618489359031386,-0.0112334529114389),
 .UNSPECIFIED.);
#358=B_SPLINE_CURVE_WITH_KNOTS('',3,(#16090,#16091,#16092,#16093),
 .UNSPECIFIED.,.F.,.F.,(4,4),(0.0112755522169305,0.618164468641375),
 .UNSPECIFIED.);
#359=B_SPLINE_CURVE_WITH_KNOTS('',3,(#16114,#16115,#16116,#16117),
 .UNSPECIFIED.,.F.,.F.,(4,4),(-0.618164468641375,-0.0112755522169305),
 .UNSPECIFIED.);
#360=B_SPLINE_CURVE_WITH_KNOTS('',3,(#16203,#16204,#16205,#16206),
 .UNSPECIFIED.,.F.,.F.,(4,4),(5.55111512312578E-17,0.618489359031386),
 .UNSPECIFIED.);
#361=B_SPLINE_CURVE_WITH_KNOTS('',3,(#16207,#16208,#16209,#16210),
 .UNSPECIFIED.,.F.,.F.,(4,4),(-0.618489359031386,-0.00110654915602034),
 .UNSPECIFIED.);
#362=B_SPLINE_CURVE_WITH_KNOTS('',3,(#16246,#16247,#16248,#16249,#16250),
 .UNSPECIFIED.,.F.,.F.,(4,1,4),(-10.4271318523291,-4.63063308449434,-0.283259008618247),
 .UNSPECIFIED.);
#363=B_SPLINE_CURVE_WITH_KNOTS('',3,(#16251,#16252,#16253,#16254,#16255),
 .UNSPECIFIED.,.F.,.F.,(4,1,4),(0.283259011433087,4.63063308449434,10.4271318523291),
 .UNSPECIFIED.);
#364=B_SPLINE_CURVE_WITH_KNOTS('',3,(#16276,#16277,#16278,#16279),
 .UNSPECIFIED.,.F.,.F.,(4,4),(0.000779732613545348,0.618164468641375),
 .UNSPECIFIED.);
#365=B_SPLINE_CURVE_WITH_KNOTS('',3,(#16280,#16281,#16282,#16283),
 .UNSPECIFIED.,.F.,.F.,(4,4),(-0.618164468641375,-4.9439619065339E-17),
 .UNSPECIFIED.);
#366=B_SPLINE_CURVE_WITH_KNOTS('',3,(#16304,#16305,#16306,#16307),
 .UNSPECIFIED.,.F.,.F.,(4,4),(3.0964814046186E-16,0.618164468641375),
 .UNSPECIFIED.);
#367=B_SPLINE_CURVE_WITH_KNOTS('',3,(#16308,#16309,#16310,#16311),
 .UNSPECIFIED.,.F.,.F.,(4,4),(-0.618164468641375,-0.0007797326135453),
 .UNSPECIFIED.);
#368=B_SPLINE_CURVE_WITH_KNOTS('',3,(#16337,#16338,#16339,#16340,#16341),
 .UNSPECIFIED.,.F.,.F.,(4,1,4),(-10.419271481025,-4.62277271319024,-0.27539863731415),
 .UNSPECIFIED.);
#369=B_SPLINE_CURVE_WITH_KNOTS('',3,(#16342,#16343,#16344,#16345,#16346),
 .UNSPECIFIED.,.F.,.F.,(4,1,4),(0.27539863731415,4.62277271319024,10.419271481025),
 .UNSPECIFIED.);
#370=B_SPLINE_CURVE_WITH_KNOTS('',3,(#16367,#16368,#16369,#16370),
 .UNSPECIFIED.,.F.,.F.,(4,4),(0.00110654915602046,0.618489359031386),
 .UNSPECIFIED.);
#371=B_SPLINE_CURVE_WITH_KNOTS('',3,(#16371,#16372,#16373,#16374),
 .UNSPECIFIED.,.F.,.F.,(4,4),(-0.618489359031386,6.93889390390723E-18),
 .UNSPECIFIED.);
#372=B_SPLINE_CURVE_WITH_KNOTS('',3,(#16416,#16417,#16418,#16419,#16420,
#16421,#16422,#16423,#16424,#16425),.UNSPECIFIED.,.F.,.F.,(4,3,3,4),(-4.09202352044852,
-3.99057144343763,-2.99292858257822,-2.07317267331971),.UNSPECIFIED.);
#373=B_SPLINE_CURVE_WITH_KNOTS('',3,(#16428,#16429,#16430,#16431,#16432,
#16433,#16434),.UNSPECIFIED.,.F.,.F.,(4,3,4),(0.,0.998042281124014,1.12274180646116),
 .UNSPECIFIED.);
#374=B_SPLINE_CURVE_WITH_KNOTS('',3,(#16439,#16440,#16441,#16442,#16443,
#16444,#16445,#16446,#16447,#16448,#16449,#16450,#16451,#16452,#16453,#16454,
#16455,#16456,#16457,#16458,#16459,#16460),.UNSPECIFIED.,.F.,.F.,(4,3,3,
3,3,3,3,4),(-10.3752088276281,-9.97642860859406,-8.97878574773466,-7.98114288687525,
-6.98350002601584,-5.98585716515644,-4.98821430429703,-4.09202352044852),
 .UNSPECIFIED.);
#375=B_SPLINE_CURVE_WITH_KNOTS('',3,(#16461,#16462,#16463,#16464,#16465,
#16466,#16467,#16468,#16469,#16470,#16471,#16472,#16473,#16474,#16475,#16476,
#16477,#16478,#16479,#16480,#16481,#16482),.UNSPECIFIED.,.F.,.F.,(4,3,3,
3,3,3,3,4),(1.12274180646116,1.99608456224804,2.99412684337208,3.99216912449611,
4.99021140562014,5.98825368674417,6.98629596786821,7.40592711364074),
 .UNSPECIFIED.);
#376=B_SPLINE_CURVE_WITH_KNOTS('',3,(#16487,#16488,#16489,#16490,#16491,
#16492,#16493,#16494,#16495,#16496,#16497,#16498,#16499,#16500,#16501,#16502,
#16503,#16504,#16505,#16506,#16507,#16508),.UNSPECIFIED.,.F.,.F.,(4,3,3,
3,3,3,3,4),(-16.6583941348077,-15.9622857737505,-14.9646429128911,-13.9670000520317,
-12.9693571911723,-11.9717143303129,-10.9740714694535,-10.3752088276281),
 .UNSPECIFIED.);
#377=B_SPLINE_CURVE_WITH_KNOTS('',3,(#16509,#16510,#16511,#16512,#16513,
#16514,#16515,#16516,#16517,#16518,#16519,#16520,#16521,#16522,#16523,#16524,
#16525,#16526,#16527,#16528,#16529,#16530),.UNSPECIFIED.,.F.,.F.,(4,3,3,
3,3,3,3,4),(7.40592711364074,7.98433824899223,8.98238053011626,9.98042281124028,
10.9784650923643,11.9765073734883,12.9745496546124,13.6891124208203),
 .UNSPECIFIED.);
#378=B_SPLINE_CURVE_WITH_KNOTS('',3,(#16535,#16536,#16537,#16538,#16539,
#16540,#16541,#16542,#16543,#16544,#16545,#16546,#16547,#16548,#16549,#16550,
#16551,#16552,#16553,#16554,#16555,#16556),.UNSPECIFIED.,.F.,.F.,(4,3,3,
3,3,3,3,4),(-22.9415794419873,-21.9481429389069,-20.9505000780475,-19.9528572171881,
-18.9552143563287,-17.9575714954693,-16.9599286346099,-16.6583941348077),
 .UNSPECIFIED.);
#379=B_SPLINE_CURVE_WITH_KNOTS('',3,(#16557,#16558,#16559,#16560,#16561,
#16562,#16563,#16564,#16565,#16566,#16567,#16568,#16569,#16570,#16571,#16572,
#16573,#16574,#16575,#16576,#16577,#16578,#16579,#16580,#16581),
 .UNSPECIFIED.,.F.,.F.,(4,3,3,3,3,3,3,3,4),(13.6891124208203,13.9725919357364,
14.9706342168604,15.9686764979844,16.9667187791085,17.9647610602325,18.9628033413565,
19.9608456224805,19.9722977279999),.UNSPECIFIED.);
#380=B_SPLINE_CURVE_WITH_KNOTS('',3,(#16586,#16587,#16588,#16589,#16590,
#16591,#16592,#16593,#16594,#16595,#16596,#16597,#16598,#16599,#16600,#16601,
#16602,#16603,#16604,#16605,#16606,#16607),.UNSPECIFIED.,.F.,.F.,(4,3,3,
3,3,3,3,4),(-29.2247647491669,-28.9316429649228,-27.9340001040634,-26.936357243204,
-25.9387143823446,-24.9410715214852,-23.9434286606257,-22.9415794419873),
 .UNSPECIFIED.);
#381=B_SPLINE_CURVE_WITH_KNOTS('',3,(#16608,#16609,#16610,#16611,#16612,
#16613,#16614,#16615,#16616,#16617,#16618,#16619,#16620,#16621,#16622,#16623,
#16624,#16625,#16626,#16627,#16628,#16629),.UNSPECIFIED.,.F.,.F.,(4,3,3,
3,3,3,3,4),(19.9722977279999,20.9588879036046,21.9569301847286,22.9549724658526,
23.9530147469767,24.9510570281007,25.9490993092247,26.2554830351795),
 .UNSPECIFIED.);
#382=B_SPLINE_CURVE_WITH_KNOTS('',3,(#16634,#16635,#16636,#16637,#16638,
#16639,#16640,#16641,#16642,#16643,#16644,#16645,#16646,#16647,#16648,#16649,
#16650,#16651,#16652,#16653,#16654,#16655),.UNSPECIFIED.,.F.,.F.,(4,3,3,
3,3,3,3,4),(-35.5079500563465,-34.9175001300792,-33.9198572692198,-32.9222144083604,
-31.924571547501,-30.9269286866416,-29.9292858257822,-29.2247647491669),
 .UNSPECIFIED.);
#383=B_SPLINE_CURVE_WITH_KNOTS('',3,(#16656,#16657,#16658,#16659,#16660,
#16661,#16662,#16663,#16664,#16665,#16666,#16667,#16668,#16669,#16670,#16671,
#16672,#16673,#16674,#16675,#16676,#16677),.UNSPECIFIED.,.F.,.F.,(4,3,3,
3,3,3,3,4),(26.2554830351795,26.9471415903487,27.9451838714728,28.9432261525968,
29.9412684337208,30.9393107148448,31.9373529959689,32.5386683423591),
 .UNSPECIFIED.);
#384=B_SPLINE_CURVE_WITH_KNOTS('',3,(#16682,#16683,#16684,#16685,#16686,
#16687,#16688,#16689,#16690,#16691,#16692,#16693,#16694,#16695,#16696,#16697,
#16698,#16699,#16700,#16701,#16702,#16703),.UNSPECIFIED.,.F.,.F.,(4,3,3,
3,3,3,3,4),(-41.791135363526,-40.9033572952357,-39.9057144343762,-38.9080715735168,
-37.9104287126574,-36.912785851798,-35.9151429909386,-35.5079500563465),
 .UNSPECIFIED.);
#385=B_SPLINE_CURVE_WITH_KNOTS('',3,(#16704,#16705,#16706,#16707,#16708,
#16709,#16710,#16711,#16712,#16713,#16714,#16715,#16716,#16717,#16718,#16719,
#16720,#16721,#16722,#16723,#16724,#16725),.UNSPECIFIED.,.F.,.F.,(4,3,3,
3,3,3,3,4),(32.5386683423591,32.9353952770929,33.9334375582169,34.931479839341,
35.929522120465,36.927564401589,37.9256066827131,38.8218536495387),
 .UNSPECIFIED.);
#386=B_SPLINE_CURVE_WITH_KNOTS('',3,(#16730,#16731,#16732,#16733,#16734,
#16735,#16736,#16737,#16738,#16739,#16740,#16741,#16742,#16743,#16744,#16745,
#16746,#16747,#16748,#16749,#16750,#16751,#16752,#16753,#16754),
 .UNSPECIFIED.,.F.,.F.,(4,3,3,3,3,3,3,3,4),(-48.0743206707056,-47.8868573212515,
-46.8892144603921,-45.8915715995327,-44.8939287386733,-43.8962858778139,
-42.8986430169545,-41.9010001560951,-41.791135363526),.UNSPECIFIED.);
#387=B_SPLINE_CURVE_WITH_KNOTS('',3,(#16755,#16756,#16757,#16758,#16759,
#16760,#16761,#16762,#16763,#16764,#16765,#16766,#16767,#16768,#16769,#16770,
#16771,#16772,#16773,#16774,#16775,#16776,#16777,#16778,#16779),
 .UNSPECIFIED.,.F.,.F.,(4,3,3,3,3,3,3,3,4),(38.8218536495387,38.9236489638371,
39.9216912449611,40.9197335260851,41.9177758072091,42.9158180883332,43.9138603694572,
44.9119026505812,45.1050389567183),.UNSPECIFIED.);
#388=B_SPLINE_CURVE_WITH_KNOTS('',3,(#16784,#16785,#16786,#16787,#16788,
#16789,#16790,#16791,#16792,#16793,#16794,#16795,#16796,#16797,#16798,#16799,
#16800,#16801,#16802,#16803,#16804,#16805),.UNSPECIFIED.,.F.,.F.,(4,3,3,
3,3,3,3,4),(-54.3575059778852,-53.8727144864079,-52.8750716255485,-51.8774287646891,
-50.8797859038297,-49.8821430429703,-48.8845001821109,-48.0743206707056),
 .UNSPECIFIED.);
#389=B_SPLINE_CURVE_WITH_KNOTS('',3,(#16806,#16807,#16808,#16809,#16810,
#16811,#16812,#16813,#16814,#16815,#16816,#16817,#16818,#16819,#16820,#16821,
#16822,#16823,#16824,#16825,#16826,#16827),.UNSPECIFIED.,.F.,.F.,(4,3,3,
3,3,3,3,4),(45.1050389567183,45.9099449317052,46.9079872128293,47.9060294939533,
48.9040717750773,49.9021140562014,50.9001563373254,51.3882242638979),
 .UNSPECIFIED.);
#390=B_SPLINE_CURVE_WITH_KNOTS('',3,(#16832,#16833,#16834,#16835,#16836,
#16837,#16838,#16839,#16840,#16841,#16842,#16843,#16844,#16845,#16846,#16847,
#16848,#16849,#16850,#16851,#16852,#16853),.UNSPECIFIED.,.F.,.F.,(4,3,3,
3,3,3,3,4),(-60.6406912850648,-59.8585716515644,-58.860928790705,-57.8632859298455,
-56.8656430689861,-55.8680002081267,-54.8703573472673,-54.3575059778852),
 .UNSPECIFIED.);
#391=B_SPLINE_CURVE_WITH_KNOTS('',3,(#16854,#16855,#16856,#16857,#16858,
#16859,#16860,#16861,#16862,#16863,#16864,#16865,#16866,#16867,#16868,#16869,
#16870,#16871,#16872,#16873,#16874,#16875),.UNSPECIFIED.,.F.,.F.,(4,3,3,
3,3,3,3,4),(51.3882242638979,51.8981986184494,52.8962408995734,53.8942831806975,
54.8923254618215,55.8903677429455,56.8884100240695,57.6714095710775),
 .UNSPECIFIED.);
#392=B_SPLINE_CURVE_WITH_KNOTS('',3,(#16880,#16881,#16882,#16883,#16884,
#16885,#16886,#16887,#16888,#16889,#16890,#16891,#16892,#16893,#16894,#16895,
#16896,#16897,#16898,#16899,#16900,#16901,#16902,#16903,#16904),
 .UNSPECIFIED.,.F.,.F.,(4,3,3,3,3,3,3,3,4),(-66.9238765922444,-66.8420716775802,
-65.8444288167208,-64.8467859558614,-63.849143095002,-62.8515002341426,
-61.8538573732832,-60.8562145124238,-60.6406912850648),.UNSPECIFIED.);
#393=B_SPLINE_CURVE_WITH_KNOTS('',3,(#16905,#16906,#16907,#16908,#16909,
#16910,#16911,#16912,#16913,#16914,#16915,#16916,#16917,#16918,#16919,#16920,
#16921,#16922,#16923,#16924,#16925,#16926,#16927,#16928,#16929),
 .UNSPECIFIED.,.F.,.F.,(4,3,3,3,3,3,3,3,4),(57.6714095710775,57.8864523051936,
58.8844945863176,59.8825368674416,60.8805791485657,61.8786214296897,62.8766637108137,
63.8747059919378,63.9545948782571),.UNSPECIFIED.);
#394=B_SPLINE_CURVE_WITH_KNOTS('',3,(#16934,#16935,#16936,#16937,#16938,
#16939,#16940,#16941,#16942,#16943,#16944,#16945,#16946,#16947,#16948,#16949,
#16950,#16951,#16952,#16953,#16954,#16955),.UNSPECIFIED.,.F.,.F.,(4,3,3,
3,3,3,3,4),(-73.207061899424,-72.8279288427366,-71.8302859818773,-70.8326431210178,
-69.8350002601584,-68.837357399299,-67.8397145384396,-66.9238765922444),
 .UNSPECIFIED.);
#395=B_SPLINE_CURVE_WITH_KNOTS('',3,(#16956,#16957,#16958,#16959,#16960,
#16961,#16962,#16963,#16964,#16965,#16966,#16967,#16968,#16969,#16970,#16971,
#16972,#16973,#16974,#16975,#16976,#16977),.UNSPECIFIED.,.F.,.F.,(4,3,3,
3,3,3,3,4),(63.9545948782571,64.8727482730618,65.8707905541858,66.8688328353098,
67.8668751164338,68.8649173975579,69.8629596786819,70.2377801854366),
 .UNSPECIFIED.);
#396=B_SPLINE_CURVE_WITH_KNOTS('',3,(#16982,#16983,#16984,#16985,#16986,
#16987,#16988,#16989,#16990,#16991,#16992,#16993,#16994,#16995,#16996,#16997,
#16998,#16999,#17000,#17001,#17002,#17003),.UNSPECIFIED.,.F.,.F.,(4,3,3,
3,3,3,3,4),(-79.4902472066036,-78.8137860078931,-77.8161431470337,-76.8185002861743,
-75.8208574253149,-74.8232145644555,-73.825571703596,-73.207061899424),
 .UNSPECIFIED.);
#397=B_SPLINE_CURVE_WITH_KNOTS('',3,(#17004,#17005,#17006,#17007,#17008,
#17009,#17010,#17011,#17012,#17013,#17014,#17015,#17016,#17017,#17018,#17019,
#17020,#17021,#17022,#17023,#17024,#17025),.UNSPECIFIED.,.F.,.F.,(4,3,3,
3,3,3,3,4),(70.2377801854366,70.8610019598059,71.85904424093,72.857086522054,
73.855128803178,74.853171084302,75.8512133654261,76.5209654926162),
 .UNSPECIFIED.);
#398=B_SPLINE_CURVE_WITH_KNOTS('',3,(#17030,#17031,#17032,#17033,#17034,
#17035,#17036,#17037,#17038,#17039,#17040,#17041,#17042,#17043,#17044,#17045,
#17046,#17047,#17048,#17049,#17050,#17051),.UNSPECIFIED.,.F.,.F.,(4,3,3,
3,3,3,3,4),(-85.7734325137832,-84.7996431730495,-83.8020003121901,-82.8043574513307,
-81.8067145904713,-80.8090717296119,-79.8114288687525,-79.4902472066036),
 .UNSPECIFIED.);
#399=B_SPLINE_CURVE_WITH_KNOTS('',3,(#17052,#17053,#17054,#17055,#17056,
#17057,#17058,#17059,#17060,#17061,#17062,#17063,#17064,#17065,#17066,#17067,
#17068,#17069,#17070,#17071,#17072,#17073),.UNSPECIFIED.,.F.,.F.,(4,3,3,
3,3,3,3,4),(76.5209654926162,76.8492556465501,77.8472979276741,78.8453402087982,
79.8433824899222,80.8414247710462,81.8394670521702,82.8041507997958),
 .UNSPECIFIED.);
#400=B_SPLINE_CURVE_WITH_KNOTS('',3,(#17078,#17079,#17080,#17081,#17082,
#17083,#17084,#17085,#17086,#17087,#17088,#17089,#17090,#17091,#17092,#17093,
#17094,#17095,#17096,#17097,#17098,#17099,#17100,#17101,#17102),
 .UNSPECIFIED.,.F.,.F.,(4,3,3,3,3,3,3,3,4),(-92.0566178209628,-91.7831431990654,
-90.7855003382059,-89.7878574773465,-88.7902146164871,-87.7925717556277,
-86.7949288947683,-85.7972860339089,-85.7734325137832),.UNSPECIFIED.);
#401=B_SPLINE_CURVE_WITH_KNOTS('',3,(#17103,#17104,#17105,#17106,#17107,
#17108,#17109,#17110,#17111,#17112,#17113,#17114,#17115,#17116,#17117,#17118,
#17119,#17120,#17121,#17122,#17123,#17124,#17125,#17126,#17127),
 .UNSPECIFIED.,.F.,.F.,(4,3,3,3,3,3,3,3,4),(82.8041507997958,82.8375093332942,
83.8355516144183,84.8335938955423,85.8316361766664,86.8296784577904,87.8277207389144,
88.8257630200384,89.0873361069754),.UNSPECIFIED.);
#402=B_SPLINE_CURVE_WITH_KNOTS('',3,(#17132,#17133,#17134,#17135,#17136,
#17137,#17138,#17139,#17140,#17141,#17142,#17143,#17144,#17145,#17146,#17147,
#17148,#17149,#17150,#17151,#17152,#17153),.UNSPECIFIED.,.F.,.F.,(4,3,3,
3,3,3,3,4),(-98.3398031281424,-97.7690003642218,-96.7713575033624,-95.773714642503,
-94.7760717816436,-93.7784289207842,-92.7807860599248,-92.0566178209628),
 .UNSPECIFIED.);
#403=B_SPLINE_CURVE_WITH_KNOTS('',3,(#17154,#17155,#17156,#17157,#17158,
#17159,#17160,#17161,#17162,#17163,#17164,#17165,#17166,#17167,#17168,#17169,
#17170,#17171,#17172,#17173,#17174,#17175),.UNSPECIFIED.,.F.,.F.,(4,3,3,
3,3,3,3,4),(89.0873361069754,89.8238053011624,90.8218475822865,91.8198898634105,
92.8179321445345,93.8159744256585,94.8140167067826,95.370521414155),
 .UNSPECIFIED.);
#404=B_SPLINE_CURVE_WITH_KNOTS('',3,(#17180,#17181,#17182,#17183,#17184,
#17185,#17186,#17187,#17188,#17189,#17190,#17191,#17192,#17193,#17194,#17195,
#17196,#17197,#17198,#17199,#17200,#17201),.UNSPECIFIED.,.F.,.F.,(4,3,3,
3,3,3,3,4),(-104.622988435322,-103.754857529378,-102.757214668519,-101.759571807659,
-100.7619289468,-99.7642860859406,-98.7666432250812,-98.3398031281424),
 .UNSPECIFIED.);
#405=B_SPLINE_CURVE_WITH_KNOTS('',3,(#17202,#17203,#17204,#17205,#17206,
#17207,#17208,#17209,#17210,#17211,#17212,#17213,#17214,#17215,#17216,#17217,
#17218,#17219,#17220,#17221,#17222,#17223),.UNSPECIFIED.,.F.,.F.,(4,3,3,
3,3,3,3,4),(95.370521414155,95.8120589879066,96.8101012690306,97.8081435501546,
98.8061858312787,99.8042281124027,100.802270393527,101.653706721335),
 .UNSPECIFIED.);
#406=B_SPLINE_CURVE_WITH_KNOTS('',3,(#17228,#17229,#17230,#17231,#17232,
#17233,#17234,#17235,#17236,#17237,#17238,#17239,#17240,#17241,#17242,#17243,
#17244,#17245,#17246,#17247,#17248,#17249,#17250,#17251,#17252),
 .UNSPECIFIED.,.F.,.F.,(4,3,3,3,3,3,3,3,4),(-110.906173742502,-110.738357555394,
-109.740714694535,-108.743071833675,-107.745428972816,-106.747786111956,
-105.750143251097,-104.752500390238,-104.622988435322),.UNSPECIFIED.);
#407=B_SPLINE_CURVE_WITH_KNOTS('',3,(#17253,#17254,#17255,#17256,#17257,
#17258,#17259,#17260,#17261,#17262,#17263,#17264,#17265,#17266,#17267,#17268,
#17269,#17270,#17271,#17272,#17273,#17274,#17275,#17276,#17277),
 .UNSPECIFIED.,.F.,.F.,(4,3,3,3,3,3,3,3,4),(101.653706721335,101.800312674651,
102.798354955775,103.796397236899,104.794439518023,105.792481799147,106.790524080271,
107.788566361395,107.936892028514),.UNSPECIFIED.);
#408=B_SPLINE_CURVE_WITH_KNOTS('',3,(#17282,#17283,#17284,#17285,#17286,
#17287,#17288,#17289,#17290,#17291,#17292,#17293,#17294,#17295,#17296,#17297,
#17298,#17299,#17300,#17301,#17302,#17303),.UNSPECIFIED.,.F.,.F.,(4,3,3,
3,3,3,3,4),(-117.189359049681,-116.724214720551,-115.726571859691,-114.728928998832,
-113.731286137972,-112.733643277113,-111.736000416253,-110.906173742502),
 .UNSPECIFIED.);
#409=B_SPLINE_CURVE_WITH_KNOTS('',3,(#17304,#17305,#17306,#17307,#17308,
#17309,#17310,#17311,#17312,#17313,#17314,#17315,#17316,#17317,#17318,#17319,
#17320,#17321,#17322,#17323,#17324,#17325),.UNSPECIFIED.,.F.,.F.,(4,3,3,
3,3,3,3,4),(107.936892028514,108.786608642519,109.784650923643,110.782693204767,
111.780735485891,112.778777767015,113.776820048139,114.220077335694),
 .UNSPECIFIED.);
#410=B_SPLINE_CURVE_WITH_KNOTS('',3,(#17330,#17331,#17332,#17333,#17334,
#17335,#17336,#17337,#17338,#17339,#17340,#17341,#17342,#17343,#17344,#17345,
#17346,#17347,#17348,#17349,#17350,#17351),.UNSPECIFIED.,.F.,.F.,(4,3,3,
3,3,3,3,4),(-123.472544356861,-122.710071885707,-121.712429024848,-120.714786163988,
-119.717143303129,-118.719500442269,-117.72185758141,-117.189359049681),
 .UNSPECIFIED.);
#411=B_SPLINE_CURVE_WITH_KNOTS('',3,(#17352,#17353,#17354,#17355,#17356,
#17357,#17358,#17359,#17360,#17361,#17362,#17363,#17364,#17365,#17366,#17367,
#17368,#17369,#17370,#17371,#17372,#17373),.UNSPECIFIED.,.F.,.F.,(4,3,3,
3,3,3,3,4),(114.220077335694,114.774862329263,115.772904610387,116.770946891511,
117.768989172635,118.767031453759,119.765073734883,120.503262642873),
 .UNSPECIFIED.);
#412=B_SPLINE_CURVE_WITH_KNOTS('',3,(#17378,#17379,#17380,#17381,#17382,
#17383,#17384,#17385,#17386,#17387,#17388,#17389,#17390,#17391,#17392,#17393,
#17394,#17395,#17396,#17397,#17398,#17399,#17400,#17401,#17402),
 .UNSPECIFIED.,.F.,.F.,(4,3,3,3,3,3,3,3,4),(-129.75572966404,-129.693571911723,
-128.695929050863,-127.698286190004,-126.700643329145,-125.703000468285,
-124.705357607426,-123.707714746566,-123.472544356861),.UNSPECIFIED.);
#413=B_SPLINE_CURVE_WITH_KNOTS('',3,(#17403,#17404,#17405,#17406,#17407,
#17408,#17409,#17410,#17411,#17412,#17413,#17414,#17415,#17416,#17417,#17418,
#17419,#17420,#17421,#17422,#17423,#17424,#17425,#17426,#17427),
 .UNSPECIFIED.,.F.,.F.,(4,3,3,3,3,3,3,3,4),(120.503262642873,120.763116016007,
121.761158297131,122.759200578255,123.757242859379,124.755285140503,125.753327421627,
126.751369702751,126.786447950053),.UNSPECIFIED.);
#414=B_SPLINE_CURVE_WITH_KNOTS('',3,(#17432,#17433,#17434,#17435,#17436,
#17437,#17438,#17439,#17440,#17441,#17442,#17443,#17444,#17445,#17446,#17447,
#17448,#17449,#17450,#17451,#17452,#17453),.UNSPECIFIED.,.F.,.F.,(4,3,3,
3,3,3,3,4),(-136.03891497122,-135.679429076879,-134.68178621602,-133.68414335516,
-132.686500494301,-131.688857633442,-130.691214772582,-129.75572966404),
 .UNSPECIFIED.);
#415=B_SPLINE_CURVE_WITH_KNOTS('',3,(#17454,#17455,#17456,#17457,#17458,
#17459,#17460,#17461,#17462,#17463,#17464,#17465,#17466,#17467,#17468,#17469,
#17470,#17471,#17472,#17473,#17474,#17475),.UNSPECIFIED.,.F.,.F.,(4,3,3,
3,3,3,3,4),(126.786447950053,127.749411983875,128.747454265,129.745496546124,
130.743538827248,131.741581108372,132.739623389496,133.069633257233),
 .UNSPECIFIED.);
#416=B_SPLINE_CURVE_WITH_KNOTS('',3,(#17480,#17481,#17482,#17483,#17484,
#17485,#17486,#17487,#17488,#17489,#17490,#17491,#17492,#17493,#17494,#17495,
#17496,#17497,#17498,#17499,#17500,#17501),.UNSPECIFIED.,.F.,.F.,(4,3,3,
3,3,3,3,4),(-142.322100278399,-141.665286242036,-140.667643381176,-139.670000520317,
-138.672357659457,-137.674714798598,-136.677071937739,-136.03891497122),
 .UNSPECIFIED.);
#417=B_SPLINE_CURVE_WITH_KNOTS('',3,(#17502,#17503,#17504,#17505,#17506,
#17507,#17508,#17509,#17510,#17511,#17512,#17513,#17514,#17515,#17516,#17517,
#17518,#17519,#17520,#17521,#17522,#17523),.UNSPECIFIED.,.F.,.F.,(4,3,3,
3,3,3,3,4),(133.069633257233,133.73766567062,134.735707951744,135.733750232868,
136.731792513992,137.729834795116,138.72787707624,139.352818564412),
 .UNSPECIFIED.);
#418=B_SPLINE_CURVE_WITH_KNOTS('',3,(#17528,#17529,#17530,#17531,#17532,
#17533,#17534,#17535,#17536,#17537,#17538,#17539,#17540,#17541,#17542,#17543,
#17544,#17545,#17546,#17547,#17548,#17549),.UNSPECIFIED.,.F.,.F.,(4,3,3,
3,3,3,3,4),(-148.605285585579,-147.651143407192,-146.653500546333,-145.655857685473,
-144.658214824614,-143.660571963754,-142.662929102895,-142.322100278399),
 .UNSPECIFIED.);
#419=B_SPLINE_CURVE_WITH_KNOTS('',3,(#17550,#17551,#17552,#17553,#17554,
#17555,#17556,#17557,#17558,#17559,#17560,#17561,#17562,#17563,#17564,#17565,
#17566,#17567,#17568,#17569,#17570,#17571),.UNSPECIFIED.,.F.,.F.,(4,3,3,
3,3,3,3,4),(139.352818564412,139.725919357364,140.723961638488,141.722003919612,
142.720046200736,143.71808848186,144.716130762984,145.636003871592),
 .UNSPECIFIED.);
#420=B_SPLINE_CURVE_WITH_KNOTS('',3,(#17576,#17577,#17578,#17579,#17580,
#17581,#17582,#17583,#17584,#17585,#17586,#17587,#17588,#17589,#17590,#17591,
#17592,#17593,#17594,#17595,#17596,#17597,#17598,#17599,#17600),
 .UNSPECIFIED.,.F.,.F.,(4,3,3,3,3,3,3,3,4),(-154.888470892759,-154.634643433208,
-153.637000572349,-152.639357711489,-151.64171485063,-150.64407198977,-149.646429128911,
-148.648786268052,-148.605285585579),.UNSPECIFIED.);
#421=B_SPLINE_CURVE_WITH_KNOTS('',3,(#17601,#17602,#17603,#17604,#17605,
#17606,#17607,#17608,#17609,#17610,#17611,#17612,#17613,#17614,#17615,#17616,
#17617,#17618,#17619,#17620,#17621,#17622,#17623,#17624,#17625),
 .UNSPECIFIED.,.F.,.F.,(4,3,3,3,3,3,3,3,4),(145.636003871592,145.714173044108,
146.712215325232,147.710257606356,148.70829988748,149.706342168604,150.704384449728,
151.702426730852,151.919189178771),.UNSPECIFIED.);
#422=B_SPLINE_CURVE_WITH_KNOTS('',3,(#17630,#17631,#17632,#17633,#17634,
#17635,#17636,#17637,#17638,#17639,#17640,#17641,#17642,#17643,#17644,#17645,
#17646,#17647,#17648,#17649,#17650,#17651),.UNSPECIFIED.,.F.,.F.,(4,3,3,
3,3,3,3,4),(-161.171656199938,-160.620500598364,-159.622857737505,-158.625214876646,
-157.627572015786,-156.629929154927,-155.632286294067,-154.888470892759),
 .UNSPECIFIED.);
#423=B_SPLINE_CURVE_WITH_KNOTS('',3,(#17652,#17653,#17654,#17655,#17656,
#17657,#17658,#17659,#17660,#17661,#17662,#17663,#17664,#17665,#17666,#17667,
#17668,#17669,#17670,#17671,#17672,#17673),.UNSPECIFIED.,.F.,.F.,(4,3,3,
3,3,3,3,4),(151.919189178771,152.700469011976,153.6985112931,154.696553574224,
155.694595855348,156.692638136472,157.690680417596,158.202374485951),
 .UNSPECIFIED.);
#424=B_SPLINE_CURVE_WITH_KNOTS('',3,(#17678,#17679,#17680,#17681,#17682,
#17683,#17684,#17685,#17686,#17687,#17688,#17689,#17690,#17691,#17692,#17693,
#17694,#17695,#17696,#17697,#17698,#17699),.UNSPECIFIED.,.F.,.F.,(4,3,3,
3,3,3,3,4),(-167.454841507118,-166.606357763521,-165.608714902661,-164.611072041802,
-163.613429180943,-162.615786320083,-161.618143459224,-161.171656199938),
 .UNSPECIFIED.);
#425=B_SPLINE_CURVE_WITH_KNOTS('',3,(#17700,#17701,#17702,#17703,#17704,
#17705,#17706,#17707,#17708,#17709,#17710,#17711,#17712,#17713,#17714,#17715,
#17716,#17717,#17718,#17719,#17720,#17721),.UNSPECIFIED.,.F.,.F.,(4,3,3,
3,3,3,3,4),(158.202374485951,158.68872269872,159.686764979844,160.684807260968,
161.682849542092,162.680891823216,163.67893410434,164.48555979313),
 .UNSPECIFIED.);
#426=B_SPLINE_CURVE_WITH_KNOTS('',3,(#17726,#17727,#17728,#17729,#17730,
#17731,#17732,#17733,#17734,#17735,#17736,#17737,#17738,#17739,#17740,#17741,
#17742,#17743,#17744,#17745,#17746,#17747,#17748,#17749,#17750),
 .UNSPECIFIED.,.F.,.F.,(4,3,3,3,3,3,3,3,4),(-173.738026814297,-173.589857789537,
-172.592214928677,-171.594572067818,-170.596929206958,-169.599286346099,
-168.60164348524,-167.60400062438,-167.454841507118),.UNSPECIFIED.);
#427=B_SPLINE_CURVE_WITH_KNOTS('',3,(#17751,#17752,#17753,#17754,#17755,
#17756,#17757,#17758,#17759,#17760,#17761,#17762,#17763,#17764,#17765,#17766,
#17767,#17768,#17769,#17770,#17771,#17772,#17773,#17774,#17775),
 .UNSPECIFIED.,.F.,.F.,(4,3,3,3,3,3,3,3,4),(164.48555979313,164.676976385465,
165.675018666588,166.673060947713,167.671103228837,168.669145509961,169.667187791085,
170.665230072209,170.76874510031),.UNSPECIFIED.);
#428=B_SPLINE_CURVE_WITH_KNOTS('',3,(#17780,#17781,#17782,#17783,#17784,
#17785,#17786,#17787,#17788,#17789,#17790,#17791,#17792,#17793,#17794,#17795,
#17796,#17797,#17798,#17799,#17800,#17801),.UNSPECIFIED.,.F.,.F.,(4,3,3,
3,3,3,3,4),(-180.021212121477,-179.575714954693,-178.578072093834,-177.580429232974,
-176.582786372115,-175.585143511255,-174.587500650396,-173.738026814297),
 .UNSPECIFIED.);
#429=B_SPLINE_CURVE_WITH_KNOTS('',3,(#17802,#17803,#17804,#17805,#17806,
#17807,#17808,#17809,#17810,#17811,#17812,#17813,#17814,#17815,#17816,#17817,
#17818,#17819,#17820,#17821,#17822,#17823),.UNSPECIFIED.,.F.,.F.,(4,3,3,
3,3,3,3,4),(170.76874510031,171.663272353333,172.661314634457,173.659356915581,
174.657399196705,175.655441477829,176.653483758953,177.051930407489),
 .UNSPECIFIED.);
#430=B_SPLINE_CURVE_WITH_KNOTS('',3,(#17828,#17829,#17830,#17831,#17832,
#17833,#17834,#17835,#17836,#17837,#17838,#17839,#17840,#17841,#17842,#17843,
#17844,#17845,#17846,#17847,#17848,#17849),.UNSPECIFIED.,.F.,.F.,(4,3,3,
3,3,3,3,4),(-186.304397428656,-185.56157211985,-184.56392925899,-183.566286398131,
-182.568643537271,-181.571000676412,-180.573357815553,-180.021212121477),
 .UNSPECIFIED.);
#431=B_SPLINE_CURVE_WITH_KNOTS('',3,(#17850,#17851,#17852,#17853,#17854,
#17855,#17856,#17857,#17858,#17859,#17860,#17861,#17862,#17863,#17864,#17865,
#17866,#17867,#17868,#17869,#17870,#17871),.UNSPECIFIED.,.F.,.F.,(4,3,3,
3,3,3,3,4),(177.051930407489,177.651526040077,178.649568321201,179.647610602325,
180.645652883449,181.643695164573,182.641737445697,183.335115714669),
 .UNSPECIFIED.);
#432=B_SPLINE_CURVE_WITH_KNOTS('',3,(#17877,#17878,#17879,#17880,#17881,
#17882,#17883,#17884,#17885,#17886),.UNSPECIFIED.,.F.,.F.,(4,1,1,1,1,1,
1,4),(197.920337176157,198.17515472821,199.172797589069,200.170440449928,
201.168083310788,202.165726171647,203.163369032507,204.161011893366),
 .UNSPECIFIED.);
#433=B_SPLINE_CURVE_WITH_KNOTS('',3,(#17889,#17890,#17891,#17892,#17893,
#17894,#17895,#17896,#17897),.UNSPECIFIED.,.F.,.F.,(4,1,1,1,1,1,4),(197.920337176157,
197.930069567874,198.928111848998,199.926154130122,200.924196411246,201.92223869237,
202.920280973494),.UNSPECIFIED.);
#434=B_SPLINE_CURVE_WITH_KNOTS('',3,(#17902,#17903,#17904,#17905,#17906,
#17907,#17908,#17909,#17910,#17911),.UNSPECIFIED.,.F.,.F.,(4,1,1,1,1,1,
1,4),(191.637151868977,192.189297563053,193.186940423913,194.184583284772,
195.182226145631,196.179869006491,197.17751186735,197.920337176157),
 .UNSPECIFIED.);
#435=B_SPLINE_CURVE_WITH_KNOTS('',3,(#17912,#17913,#17914,#17915,#17916,
#17917,#17918,#17919,#17920,#17921),.UNSPECIFIED.,.F.,.F.,(4,1,1,1,1,1,
1,4),(191.637151868977,191.94181588113,192.939858162254,193.937900443378,
194.935942724502,195.933985005626,196.93202728675,197.920337176157),
 .UNSPECIFIED.);
#436=B_SPLINE_CURVE_WITH_KNOTS('',3,(#17926,#17927,#17928,#17929,#17930,
#17931,#17932,#17933,#17934,#17935),.UNSPECIFIED.,.F.,.F.,(4,1,1,1,1,1,
1,4),(185.353966561798,186.203440397897,187.201083258756,188.198726119616,
189.196368980475,190.194011841334,191.191654702194,191.637151868977),
 .UNSPECIFIED.);
#437=B_SPLINE_CURVE_WITH_KNOTS('',3,(#17936,#17937,#17938,#17939,#17940,
#17941,#17942,#17943,#17944,#17945),.UNSPECIFIED.,.F.,.F.,(4,1,1,1,1,1,
1,4),(185.353966561798,185.953562194385,186.951604475509,187.949646756633,
188.947689037757,189.945731318881,190.943773600006,191.637151868977),
 .UNSPECIFIED.);
#438=B_SPLINE_CURVE_WITH_KNOTS('',3,(#17950,#17951,#17952,#17953,#17954,
#17955,#17956,#17957,#17958,#17959,#17960),.UNSPECIFIED.,.F.,.F.,(4,1,1,
1,1,1,1,1,4),(179.070781254618,179.219940371881,180.21758323274,181.2152260936,
182.212868954459,183.210511815318,184.208154676178,185.205797537037,185.353966561798),
 .UNSPECIFIED.);
#439=B_SPLINE_CURVE_WITH_KNOTS('',3,(#17961,#17962,#17963,#17964,#17965,
#17966,#17967,#17968,#17969,#17970),.UNSPECIFIED.,.F.,.F.,(4,1,1,1,1,1,
1,4),(179.070781254618,179.965308507641,180.963350788765,181.961393069889,
182.959435351013,183.957477632137,184.955519913261,185.353966561798),
 .UNSPECIFIED.);
#440=B_SPLINE_CURVE_WITH_KNOTS('',3,(#17975,#17976,#17977,#17978,#17979,
#17980,#17981,#17982,#17983,#17984),.UNSPECIFIED.,.F.,.F.,(4,1,1,1,1,1,
1,4),(172.787595947439,173.234083206724,174.231726067584,175.229368928443,
176.227011789303,177.224654650162,178.222297511021,179.070781254618),
 .UNSPECIFIED.);
#441=B_SPLINE_CURVE_WITH_KNOTS('',3,(#17985,#17986,#17987,#17988,#17989,
#17990,#17991,#17992,#17993,#17994,#17995),.UNSPECIFIED.,.F.,.F.,(4,1,1,
1,1,1,1,1,4),(172.787595947439,172.979012539773,173.977054820897,174.975097102021,
175.973139383145,176.971181664269,177.969223945393,178.967266226517,179.070781254618),
 .UNSPECIFIED.);
#442=B_SPLINE_CURVE_WITH_KNOTS('',3,(#18000,#18001,#18002,#18003,#18004,
#18005,#18006,#18007,#18008,#18009),.UNSPECIFIED.,.F.,.F.,(4,1,1,1,1,1,
1,4),(166.504410640259,167.248226041568,168.245868902427,169.243511763287,
170.241154624146,171.238797485006,172.236440345865,172.787595947439),
 .UNSPECIFIED.);
#443=B_SPLINE_CURVE_WITH_KNOTS('',3,(#18010,#18011,#18012,#18013,#18014,
#18015,#18016,#18017,#18018,#18019),.UNSPECIFIED.,.F.,.F.,(4,1,1,1,1,1,
1,4),(166.504410640259,166.990758853029,167.988801134153,168.986843415277,
169.984885696401,170.982927977525,171.980970258649,172.787595947439),
 .UNSPECIFIED.);
#444=B_SPLINE_CURVE_WITH_KNOTS('',3,(#18024,#18025,#18026,#18027,#18028,
#18029,#18030,#18031,#18032,#18033,#18034),.UNSPECIFIED.,.F.,.F.,(4,1,1,
1,1,1,1,1,4),(160.22122533308,160.264726015552,161.262368876412,162.260011737271,
163.25765459813,164.25529745899,165.252940319849,166.250583180709,166.504410640259),
 .UNSPECIFIED.);
#445=B_SPLINE_CURVE_WITH_KNOTS('',3,(#18035,#18036,#18037,#18038,#18039,
#18040,#18041,#18042,#18043,#18044),.UNSPECIFIED.,.F.,.F.,(4,1,1,1,1,1,
1,4),(160.22122533308,161.002505166285,162.000547447409,162.998589728533,
163.996632009657,164.994674290781,165.992716571905,166.504410640259),
 .UNSPECIFIED.);
#446=B_SPLINE_CURVE_WITH_KNOTS('',3,(#18049,#18050,#18051,#18052,#18053,
#18054,#18055,#18056,#18057,#18058),.UNSPECIFIED.,.F.,.F.,(4,1,1,1,1,1,
1,4),(153.9380400259,154.278868850396,155.276511711255,156.274154572115,
157.271797432974,158.269440293833,159.267083154693,160.22122533308),
 .UNSPECIFIED.);
#447=B_SPLINE_CURVE_WITH_KNOTS('',3,(#18059,#18060,#18061,#18062,#18063,
#18064,#18065,#18066,#18067,#18068,#18069),.UNSPECIFIED.,.F.,.F.,(4,1,1,
1,1,1,1,1,4),(153.9380400259,154.016209198417,155.014251479541,156.012293760665,
157.010336041789,158.008378322913,159.006420604037,160.004462885161,160.22122533308),
 .UNSPECIFIED.);
#448=B_SPLINE_CURVE_WITH_KNOTS('',3,(#18074,#18075,#18076,#18077,#18078,
#18079,#18080,#18081,#18082,#18083),.UNSPECIFIED.,.F.,.F.,(4,1,1,1,1,1,
1,4),(147.65485471872,148.293011685239,149.290654546099,150.288297406958,
151.285940267817,152.283583128677,153.281225989536,153.9380400259),
 .UNSPECIFIED.);
#449=B_SPLINE_CURVE_WITH_KNOTS('',3,(#18084,#18085,#18086,#18087,#18088,
#18089,#18090,#18091,#18092,#18093),.UNSPECIFIED.,.F.,.F.,(4,1,1,1,1,1,
1,4),(147.65485471872,148.027955511672,149.025997792796,150.02404007392,
151.022082355044,152.020124636168,153.018166917292,153.9380400259),
 .UNSPECIFIED.);
#450=B_SPLINE_CURVE_WITH_KNOTS('',3,(#18098,#18099,#18100,#18101,#18102,
#18103,#18104,#18105,#18106,#18107),.UNSPECIFIED.,.F.,.F.,(4,1,1,1,1,1,
1,4),(141.371669411541,142.307154520083,143.304797380942,144.302440241802,
145.300083102661,146.29772596352,147.29536882438,147.65485471872),
 .UNSPECIFIED.);
#451=B_SPLINE_CURVE_WITH_KNOTS('',3,(#18108,#18109,#18110,#18111,#18112,
#18113,#18114,#18115,#18116,#18117),.UNSPECIFIED.,.F.,.F.,(4,1,1,1,1,1,
1,4),(141.371669411541,142.039701824928,143.037744106052,144.035786387176,
145.0338286683,146.031870949424,147.029913230548,147.65485471872),
 .UNSPECIFIED.);
#452=B_SPLINE_CURVE_WITH_KNOTS('',3,(#18122,#18123,#18124,#18125,#18126,
#18127,#18128,#18129,#18130,#18131,#18132),.UNSPECIFIED.,.F.,.F.,(4,1,1,
1,1,1,1,1,4),(135.088484104361,135.323654494067,136.321297354926,137.318940215786,
138.316583076645,139.314225937505,140.311868798364,141.309511659223,141.371669411541),
 .UNSPECIFIED.);
#453=B_SPLINE_CURVE_WITH_KNOTS('',3,(#18133,#18134,#18135,#18136,#18137,
#18138,#18139,#18140,#18141,#18142),.UNSPECIFIED.,.F.,.F.,(4,1,1,1,1,1,
1,4),(135.088484104361,136.051448138184,137.049490419308,138.047532700432,
139.045574981556,140.04361726268,141.041659543804,141.371669411541),
 .UNSPECIFIED.);
#454=B_SPLINE_CURVE_WITH_KNOTS('',3,(#18147,#18148,#18149,#18150,#18151,
#18152,#18153,#18154,#18155,#18156),.UNSPECIFIED.,.F.,.F.,(4,1,1,1,1,1,
1,4),(128.805298797182,129.337797328911,130.33544018977,131.333083050629,
132.330725911489,133.328368772348,134.326011633208,135.088484104361),
 .UNSPECIFIED.);
#455=B_SPLINE_CURVE_WITH_KNOTS('',3,(#18157,#18158,#18159,#18160,#18161,
#18162,#18163,#18164,#18165,#18166,#18167),.UNSPECIFIED.,.F.,.F.,(4,1,1,
1,1,1,1,1,4),(128.805298797182,129.065152170316,130.06319445144,131.061236732564,
132.059279013688,133.057321294812,134.055363575936,135.05340585706,135.088484104361),
 .UNSPECIFIED.);
#456=B_SPLINE_CURVE_WITH_KNOTS('',3,(#18172,#18173,#18174,#18175,#18176,
#18177,#18178,#18179,#18180,#18181),.UNSPECIFIED.,.F.,.F.,(4,1,1,1,1,1,
1,4),(122.522113490002,123.351940163754,124.349583024614,125.347225885473,
126.344868746332,127.342511607192,128.340154468051,128.805298797182),
 .UNSPECIFIED.);
#457=B_SPLINE_CURVE_WITH_KNOTS('',3,(#18182,#18183,#18184,#18185,#18186,
#18187,#18188,#18189,#18190,#18191),.UNSPECIFIED.,.F.,.F.,(4,1,1,1,1,1,
1,4),(122.522113490002,123.076898483572,124.074940764696,125.07298304582,
126.071025326944,127.069067608068,128.067109889192,128.805298797182),
 .UNSPECIFIED.);
#458=B_SPLINE_CURVE_WITH_KNOTS('',3,(#18196,#18197,#18198,#18199,#18200,
#18201,#18202,#18203,#18204,#18205,#18206),.UNSPECIFIED.,.F.,.F.,(4,1,1,
1,1,1,1,1,4),(116.238928182823,116.368440137738,117.366082998598,118.363725859457,
119.361368720316,120.359011581176,121.356654442035,122.354297302895,122.522113490002),
 .UNSPECIFIED.);
#459=B_SPLINE_CURVE_WITH_KNOTS('',3,(#18207,#18208,#18209,#18210,#18211,
#18212,#18213,#18214,#18215,#18216),.UNSPECIFIED.,.F.,.F.,(4,1,1,1,1,1,
1,4),(116.238928182823,117.088644796828,118.086687077952,119.084729359076,
120.0827716402,121.080813921324,122.078856202448,122.522113490002),
 .UNSPECIFIED.);
#460=B_SPLINE_CURVE_WITH_KNOTS('',3,(#18221,#18222,#18223,#18224,#18225,
#18226,#18227,#18228,#18229,#18230),.UNSPECIFIED.,.F.,.F.,(4,1,1,1,1,1,
1,4),(109.955742875643,110.382582972582,111.380225833441,112.377868694301,
113.37551155516,114.373154416019,115.370797276879,116.238928182823),
 .UNSPECIFIED.);
#461=B_SPLINE_CURVE_WITH_KNOTS('',3,(#18231,#18232,#18233,#18234,#18235,
#18236,#18237,#18238,#18239,#18240,#18241),.UNSPECIFIED.,.F.,.F.,(4,1,1,
1,1,1,1,1,4),(109.955742875643,110.102348828959,111.100391110083,112.098433391207,
113.096475672331,114.094517953455,115.092560234579,116.090602515703,116.238928182823),
 .UNSPECIFIED.);
#462=B_SPLINE_CURVE_WITH_KNOTS('',3,(#18246,#18247,#18248,#18249,#18250,
#18251,#18252,#18253,#18254,#18255),.UNSPECIFIED.,.F.,.F.,(4,1,1,1,1,1,
1,4),(103.672557568463,104.396725807425,105.394368668285,106.392011529144,
107.389654390004,108.387297250863,109.384940111722,109.955742875643),
 .UNSPECIFIED.);
#463=B_SPLINE_CURVE_WITH_KNOTS('',3,(#18256,#18257,#18258,#18259,#18260,
#18261,#18262,#18263,#18264,#18265),.UNSPECIFIED.,.F.,.F.,(4,1,1,1,1,1,
1,4),(103.672557568463,104.114095142215,105.112137423339,106.110179704463,
107.108221985587,108.106264266711,109.104306547835,109.955742875643),
 .UNSPECIFIED.);
#464=B_SPLINE_CURVE_WITH_KNOTS('',3,(#18270,#18271,#18272,#18273,#18274,
#18275,#18276,#18277,#18278,#18279,#18280),.UNSPECIFIED.,.F.,.F.,(4,1,1,
1,1,1,1,1,4),(97.3893722612837,97.4132257814096,98.410868642269,99.4085115031284,
100.406154363988,101.403797224847,102.401440085707,103.399082946566,103.672557568463),
 .UNSPECIFIED.);
#465=B_SPLINE_CURVE_WITH_KNOTS('',3,(#18281,#18282,#18283,#18284,#18285,
#18286,#18287,#18288,#18289,#18290),.UNSPECIFIED.,.F.,.F.,(4,1,1,1,1,1,
1,4),(97.3893722612838,98.125841455471,99.123883736595,100.121926017719,
101.119968298843,102.118010579967,103.116052861091,103.672557568463),
 .UNSPECIFIED.);
#466=B_SPLINE_CURVE_WITH_KNOTS('',3,(#18295,#18296,#18297,#18298,#18299,
#18300,#18301,#18302,#18303,#18304),.UNSPECIFIED.,.F.,.F.,(4,1,1,1,1,1,
1,4),(91.1061869541041,91.4273686162531,92.4250114771125,93.4226543379719,
94.4202971988313,95.4179400596907,96.4155829205502,97.3893722612837),
 .UNSPECIFIED.);
#467=B_SPLINE_CURVE_WITH_KNOTS('',3,(#18305,#18306,#18307,#18308,#18309,
#18310,#18311,#18312,#18313,#18314,#18315),.UNSPECIFIED.,.F.,.F.,(4,1,1,
1,1,1,1,1,4),(91.1061869541042,91.1395454876028,92.1375877687268,93.1356300498508,
94.1336723309749,95.1317146120989,96.1297568932229,97.127799174347,97.3893722612838),
 .UNSPECIFIED.);
#468=B_SPLINE_CURVE_WITH_KNOTS('',3,(#18320,#18321,#18322,#18323,#18324,
#18325,#18326,#18327,#18328,#18329),.UNSPECIFIED.,.F.,.F.,(4,1,1,1,1,1,
1,4),(84.8230016469245,85.4415114510967,86.4391543119561,87.4367971728155,
88.4344400336749,89.4320828945343,90.4297257553937,91.1061869541041),
 .UNSPECIFIED.);
#469=B_SPLINE_CURVE_WITH_KNOTS('',3,(#18330,#18331,#18332,#18333,#18334,
#18335,#18336,#18337,#18338,#18339),.UNSPECIFIED.,.F.,.F.,(4,1,1,1,1,1,
1,4),(84.8230016469246,85.1512918008586,86.1493340819827,87.1473763631067,
88.1454186442307,89.1434609253548,90.1415032064788,91.1061869541042),
 .UNSPECIFIED.);
#470=B_SPLINE_CURVE_WITH_KNOTS('',3,(#18344,#18345,#18346,#18347,#18348,
#18349,#18350,#18351,#18352,#18353),.UNSPECIFIED.,.F.,.F.,(4,1,1,1,1,1,
1,4),(78.539816339745,79.4556542859402,80.4532971467996,81.4509400076591,
82.4485828685185,83.4462257293779,84.4438685902373,84.8230016469245),
 .UNSPECIFIED.);
#471=B_SPLINE_CURVE_WITH_KNOTS('',3,(#18354,#18355,#18356,#18357,#18358,
#18359,#18360,#18361,#18362,#18363),.UNSPECIFIED.,.F.,.F.,(4,1,1,1,1,1,
1,4),(78.539816339745,79.1630381141145,80.1610803952385,81.1591226763625,
82.1571649574865,83.1552072386106,84.1532495197346,84.8230016469246),
 .UNSPECIFIED.);
#472=B_SPLINE_CURVE_WITH_KNOTS('',3,(#18368,#18369,#18370,#18371,#18372,
#18373,#18374,#18375,#18376,#18377,#18378),.UNSPECIFIED.,.F.,.F.,(4,1,1,
1,1,1,1,1,4),(72.2566310325654,72.4721542599244,73.4697971207838,74.4674399816432,
75.4650828425026,76.462725703362,77.4603685642214,78.4580114250808,78.539816339745),
 .UNSPECIFIED.);
#473=B_SPLINE_CURVE_WITH_KNOTS('',3,(#18379,#18380,#18381,#18382,#18383,
#18384,#18385,#18386,#18387,#18388),.UNSPECIFIED.,.F.,.F.,(4,1,1,1,1,1,
1,4),(72.2566310325654,73.1747844273703,74.1728267084943,75.1708689896184,
76.1689112707424,77.1669535518664,78.1649958329905,78.539816339745),
 .UNSPECIFIED.);
#474=B_SPLINE_CURVE_WITH_KNOTS('',3,(#18393,#18394,#18395,#18396,#18397,
#18398,#18399,#18400,#18401,#18402),.UNSPECIFIED.,.F.,.F.,(4,1,1,1,1,1,
1,4),(65.9734457253858,66.486297094768,67.4839399556274,68.4815828164868,
69.4792256773462,70.4768685382056,71.474511399065,72.2566310325654),
 .UNSPECIFIED.);
#475=B_SPLINE_CURVE_WITH_KNOTS('',3,(#18403,#18404,#18405,#18406,#18407,
#18408,#18409,#18410,#18411,#18412,#18413),.UNSPECIFIED.,.F.,.F.,(4,1,1,
1,1,1,1,1,4),(65.9734457253858,66.1884884595021,67.1865307406262,68.1845730217502,
69.1826153028742,70.1806575839982,71.1786998651223,72.1767421462463,72.2566310325654),
 .UNSPECIFIED.);
#476=B_SPLINE_CURVE_WITH_KNOTS('',3,(#18418,#18419,#18420,#18421,#18422,
#18423,#18424,#18425,#18426,#18427),.UNSPECIFIED.,.F.,.F.,(4,1,1,1,1,1,
1,4),(59.6902604182062,60.5004399296115,61.4980827904709,62.4957256513303,
63.4933685121897,64.4910113730492,65.4886542339086,65.9734457253858),
 .UNSPECIFIED.);
#477=B_SPLINE_CURVE_WITH_KNOTS('',3,(#18428,#18429,#18430,#18431,#18432,
#18433,#18434,#18435,#18436,#18437),.UNSPECIFIED.,.F.,.F.,(4,1,1,1,1,1,
1,4),(59.6902604182062,60.200234772758,61.198277053882,62.196319335006,
63.19436161613,64.1924038972541,65.1904461783781,65.9734457253858),
 .UNSPECIFIED.);
#478=B_SPLINE_CURVE_WITH_KNOTS('',3,(#18442,#18443,#18444,#18445,#18446,
#18447,#18448,#18449,#18450,#18451,#18452),.UNSPECIFIED.,.F.,.F.,(4,1,1,
1,1,1,1,1,4),(53.4070751110266,53.5169399035957,54.5145827644551,55.5122256253145,
56.5098684861739,57.5075113470333,58.5051542078927,59.5027970687521,59.6902604182062),
 .UNSPECIFIED.);
#479=B_SPLINE_CURVE_WITH_KNOTS('',3,(#18453,#18454,#18455,#18456,#18457,
#18458,#18459,#18460,#18461,#18462),.UNSPECIFIED.,.F.,.F.,(4,1,1,1,1,1,
1,4),(53.4070751110266,54.2119810860138,55.2100233671378,56.2080656482619,
57.2061079293859,58.2041502105099,59.2021924916339,59.6902604182062),
 .UNSPECIFIED.);
#480=B_SPLINE_CURVE_WITH_KNOTS('',3,(#18467,#18468,#18469,#18470,#18471,
#18472,#18473,#18474,#18475,#18476),.UNSPECIFIED.,.F.,.F.,(4,1,1,1,1,1,
1,4),(47.123889803847,47.5310827384393,48.5287255992987,49.5263684601581,
50.5240113210175,51.5216541818769,52.5192970427363,53.4070751110266),
 .UNSPECIFIED.);
#481=B_SPLINE_CURVE_WITH_KNOTS('',3,(#18477,#18478,#18479,#18480,#18481,
#18482,#18483,#18484,#18485,#18486,#18487),.UNSPECIFIED.,.F.,.F.,(4,1,1,
1,1,1,1,1,4),(47.123889803847,47.2256851181456,48.2237273992696,49.2217696803937,
50.2198119615177,51.2178542426417,52.2158965237657,53.2139388048898,53.4070751110266),
 .UNSPECIFIED.);
#482=B_SPLINE_CURVE_WITH_KNOTS('',3,(#18492,#18493,#18494,#18495,#18496,
#18497,#18498,#18499,#18500,#18501),.UNSPECIFIED.,.F.,.F.,(4,1,1,1,1,1,
1,4),(40.8407044966674,41.5452255732828,42.5428684341422,43.5405112950016,
44.538154155861,45.5357970167204,46.5334398775799,47.123889803847),
 .UNSPECIFIED.);
#483=B_SPLINE_CURVE_WITH_KNOTS('',3,(#18502,#18503,#18504,#18505,#18506,
#18507,#18508,#18509,#18510,#18511),.UNSPECIFIED.,.F.,.F.,(4,1,1,1,1,1,
1,4),(40.8407044966675,41.2374314314014,42.2354737125255,43.2335159936495,
44.2315582747735,45.2296005558975,46.2276428370216,47.123889803847),
 .UNSPECIFIED.);
#484=B_SPLINE_CURVE_WITH_KNOTS('',3,(#18516,#18517,#18518,#18519,#18520,
#18521,#18522,#18523,#18524,#18525,#18526),.UNSPECIFIED.,.F.,.F.,(4,1,1,
1,1,1,1,1,4),(34.5575191894878,34.561725547267,35.5593684081264,36.5570112689858,
37.5546541298452,38.5522969907046,39.549939851564,40.5475827124234,40.8407044966674),
 .UNSPECIFIED.);
#485=B_SPLINE_CURVE_WITH_KNOTS('',3,(#18527,#18528,#18529,#18530,#18531,
#18532,#18533,#18534,#18535,#18536),.UNSPECIFIED.,.F.,.F.,(4,1,1,1,1,1,
1,4),(34.5575191894879,35.2491777446573,36.2472200257813,37.2452623069053,
38.2433045880294,39.2413468691534,40.2393891502774,40.8407044966675),
 .UNSPECIFIED.);
#486=B_SPLINE_CURVE_WITH_KNOTS('',3,(#18541,#18542,#18543,#18544,#18545,
#18546,#18547,#18548,#18549,#18550),.UNSPECIFIED.,.F.,.F.,(4,1,1,1,1,1,
1,4),(28.2743338823082,28.5758683821105,29.5735112429699,30.5711541038294,
31.5687969646888,32.5664398255482,33.5640826864076,34.5575191894878),
 .UNSPECIFIED.);
#487=B_SPLINE_CURVE_WITH_KNOTS('',3,(#18551,#18552,#18553,#18554,#18555,
#18556,#18557,#18558,#18559,#18560),.UNSPECIFIED.,.F.,.F.,(4,1,1,1,1,1,
1,4),(28.2743338823083,29.2609240579131,30.2589663390371,31.2570086201612,
32.2550509012852,33.2530931824092,34.2511354635333,34.5575191894879),
 .UNSPECIFIED.);
#488=B_SPLINE_CURVE_WITH_KNOTS('',3,(#18565,#18566,#18567,#18568,#18569,
#18570,#18571,#18572,#18573,#18574),.UNSPECIFIED.,.F.,.F.,(4,1,1,1,1,1,
1,4),(21.9911485751286,22.5900112169541,23.5876540778135,24.5852969386729,
25.5829397995323,26.5805826603917,27.5782255212511,28.2743338823082),
 .UNSPECIFIED.);
#489=B_SPLINE_CURVE_WITH_KNOTS('',3,(#18575,#18576,#18577,#18578,#18579,
#18580,#18581,#18582,#18583,#18584,#18585),.UNSPECIFIED.,.F.,.F.,(4,1,1,
1,1,1,1,1,4),(21.9911485751287,22.2746280900449,23.272670371169,24.270712652293,
25.268754933417,26.266797214541,27.2648394956651,28.2628817767891,28.2743338823083),
 .UNSPECIFIED.);
#490=B_SPLINE_CURVE_WITH_KNOTS('',3,(#18590,#18591,#18592,#18593,#18594,
#18595,#18596,#18597,#18598,#18599),.UNSPECIFIED.,.F.,.F.,(4,1,1,1,1,1,
1,4),(15.707963267949,16.6041540517977,17.6017969126571,18.5994397735165,
19.5970826343759,20.5947254952353,21.5923683560947,21.9911485751286),
 .UNSPECIFIED.);
#491=B_SPLINE_CURVE_WITH_KNOTS('',3,(#18600,#18601,#18602,#18603,#18604,
#18605,#18606,#18607,#18608,#18609),.UNSPECIFIED.,.F.,.F.,(4,1,1,1,1,1,
1,4),(15.7079632679491,16.2863744033008,17.2844166844248,18.2824589655488,
19.2805012466728,20.2785435277969,21.2765858089209,21.9911485751287),
 .UNSPECIFIED.);
#492=B_SPLINE_CURVE_WITH_KNOTS('',3,(#18612,#18613,#18614,#18615,#18616,
#18617,#18618,#18619,#18620,#18621,#18622,#18623,#18624,#18625,#18626,#18627,
#18628,#18629,#18630,#18631,#18632,#18633,#18634,#18635,#18636,#18637,#18638,
#18639,#18640,#18641,#18642,#18643,#18644,#18645,#18646,#18647,#18648,#18649,
#18650,#18651,#18652,#18653,#18654,#18655,#18656,#18657,#18658,#18659,#18660,
#18661,#18662,#18663,#18664,#18665,#18666,#18667,#18668,#18669,#18670,#18671,
#18672,#18673,#18674,#18675,#18676,#18677,#18678,#18679,#18680,#18681,#18682,
#18683,#18684,#18685,#18686,#18687,#18688,#18689,#18690,#18691,#18692,#18693,
#18694,#18695,#18696,#18697,#18698,#18699,#18700,#18701,#18702,#18703,#18704,
#18705,#18706,#18707,#18708,#18709,#18710,#18711,#18712,#18713,#18714,#18715,
#18716,#18717,#18718,#18719,#18720,#18721,#18722,#18723,#18724,#18725,#18726,
#18727,#18728,#18729,#18730,#18731,#18732),.UNSPECIFIED.,.F.,.F.,(4,3,3,
3,3,3,3,3,3,3,3,3,3,3,3,3,3,3,3,3,3,3,3,3,3,3,3,3,3,3,3,3,3,3,3,3,3,3,3,
3,4),(-0.753008129282056,-0.726412283548368,-0.715911613874471,-0.694893371653716,
-0.683361029549332,-0.673826434412814,-0.652889016486892,-0.639679181765185,
-0.63195159856097,-0.60480408471638,-0.59150990338668,-0.582561183693184,
-0.554067746128576,-0.540494882749548,-0.528208608719221,-0.505843484121927,
-0.4921308028701,-0.483102814228457,-0.456032674248847,-0.436199115577779,
-0.427073928162626,-0.400948091236321,-0.382860905241332,-0.374822254310016,
-0.34584221065474,-0.333939649620793,-0.324058619604945,-0.29393738163796,
-0.278576588250954,-0.269234263278142,-0.238815915606663,-0.225742435796944,
-0.216239773488962,-0.18666367230127,-0.170750005528772,-0.161294486761502,
-0.129614927749849,-0.114924930935507,-0.106250072717365,-0.0979353687381955,
-0.0965360155478562),.UNSPECIFIED.);
#493=B_SPLINE_CURVE_WITH_KNOTS('',3,(#18734,#18735,#18736,#18737,#18738,
#18739,#18740,#18741,#18742,#18743,#18744,#18745,#18746,#18747,#18748,#18749,
#18750,#18751,#18752,#18753,#18754,#18755,#18756,#18757,#18758,#18759,#18760,
#18761,#18762,#18763,#18764,#18765,#18766,#18767,#18768,#18769,#18770),
 .UNSPECIFIED.,.F.,.F.,(4,3,3,3,3,3,3,3,3,3,3,3,4),(-0.204609524178132,
-0.173922074105667,-0.152149392827302,-0.142793959810126,-0.12983323009626,
-0.11308637627832,-0.0998536142809363,-0.090547498816978,-0.0679106241127335,
-0.0514558350659385,-0.042025593252969,-0.0155529233063705,0.),
 .UNSPECIFIED.);
#494=B_SPLINE_CURVE_WITH_KNOTS('',3,(#18773,#18774,#18775,#18776,#18777,
#18778,#18779,#18780,#18781,#18782,#18783,#18784,#18785,#18786,#18787,#18788),
 .UNSPECIFIED.,.F.,.F.,(4,3,3,3,3,4),(-0.0965360155478562,-0.0724020116608921,
-0.0590232605257019,-0.050388474335024,-0.0186937936910934,0.),
 .UNSPECIFIED.);
#495=B_SPLINE_CURVE_WITH_KNOTS('',3,(#19577,#19578,#19579,#19580,#19581,
#19582,#19583,#19584),.UNSPECIFIED.,.F.,.F.,(4,1,1,1,1,4),(11.6159397475006,
12.61358260836,13.6112254692194,14.6088683300789,15.6065111909383,15.707963267949),
 .UNSPECIFIED.);
#496=B_SPLINE_CURVE_WITH_KNOTS('',3,(#19585,#19586,#19587,#19588,#19589,
#19590,#19591,#19592,#19593,#19594,#19595,#19596,#19597,#19598,#19599,#19600,
#19601,#19602,#19603,#19604,#19605,#19606,#19607,#19608,#19609,#19610,#19611,
#19612,#19613,#19614,#19615,#19616,#19617,#19618,#19619,#19620,#19621,#19622,
#19623,#19624,#19625,#19626,#19627,#19628,#19629,#19630,#19631,#19632,#19633),
 .UNSPECIFIED.,.F.,.F.,(4,3,3,3,3,3,3,3,3,3,3,3,3,3,3,3,4),(-0.275362278356892,
-0.263988733943187,-0.242277787653762,-0.228409792083558,-0.208856161945484,
-0.197709057767663,-0.168075464588018,-0.150222803571495,-0.140083955862437,
-0.125365894046572,-0.0997819296507484,-0.0889593225835958,-0.0667194919376969,
-0.0511923416312717,-0.0404361839568205,-0.0141940669149386,0.),
 .UNSPECIFIED.);
#497=B_SPLINE_CURVE_WITH_KNOTS('',3,(#19634,#19635,#19636,#19637,#19638,
#19639,#19640,#19641,#19642,#19643,#19644,#19645,#19646,#19647,#19648,#19649,
#19650,#19651,#19652),.UNSPECIFIED.,.F.,.F.,(4,3,3,3,3,3,4),(-191.027404416132,
-190.549786424147,-189.552143563287,-188.554500702428,-187.556857841568,
-186.559214980709,-186.304397428656),.UNSPECIFIED.);
#498=B_SPLINE_CURVE_WITH_KNOTS('',3,(#19655,#19656,#19657,#19658,#19659,
#19660,#19661,#19662,#19663),.UNSPECIFIED.,.F.,.F.,(4,1,1,1,1,1,4),(10.3752088276283,
11.2961629976806,12.2942052788047,13.2922475599287,14.2902898410527,15.2883321221767,
15.7079632679491),.UNSPECIFIED.);
#499=B_SPLINE_CURVE_WITH_KNOTS('',3,(#20457,#20458,#20459,#20460,#20461,
#20462,#20463,#20464,#20465,#20466,#20467,#20468,#20469,#20470,#20471,#20472,
#20473,#20474,#20475,#20476,#20477,#20478),.UNSPECIFIED.,.F.,.F.,(4,3,3,
3,3,3,3,4),(183.335115714669,183.639779726821,184.637822007945,185.635864289069,
186.633906570193,187.631948851317,188.629991132441,188.954231742812),
 .UNSPECIFIED.);
#500=B_SPLINE_CURVE_WITH_KNOTS('',3,(#20479,#20480,#20481,#20482,#20483,
#20484,#20485,#20486,#20487,#20488,#20489,#20490,#20491,#20492,#20493,#20494,
#20495,#20496,#20497,#20498,#20499,#20500,#20501,#20502,#20503,#20504,#20505,
#20506,#20507,#20508,#20509,#20510,#20511,#20512,#20513,#20514,#20515,#20516,
#20517,#20518,#20519,#20520,#20521,#20522,#20523,#20524,#20525,#20526,#20527,
#20528,#20529,#20530),.UNSPECIFIED.,.F.,.F.,(4,3,3,3,3,3,3,3,3,3,3,3,3,
3,3,3,3,4),(-0.276631791712714,-0.267404104599176,-0.245529112929484,-0.233826742508505,
-0.212230201958684,-0.201819484750363,-0.173281546649687,-0.162756755581661,
-0.152537502224722,-0.140478169692516,-0.120739781640826,-0.110641775261762,
-0.100726383882944,-0.0755447879122082,-0.0587891884452614,-0.0493012364577666,
-0.0182848522583483,0.),.UNSPECIFIED.);
#501=B_SPLINE_CURVE_WITH_KNOTS('',3,(#20585,#20586,#20587,#20588,#20589,
#20590,#20591),.UNSPECIFIED.,.F.,.F.,(4,3,4),(-30.159289474462,-29.2544199692899,
-28.9853432330879),.UNSPECIFIED.);
#502=B_SPLINE_CURVE_WITH_KNOTS('',3,(#20597,#20598,#20599,#20600,#20601,
#20602,#20603,#20604,#20605,#20606,#20607,#20608,#20609,#20610,#20611,#20612,
#20613,#20614,#20615),.UNSPECIFIED.,.F.,.F.,(4,3,3,3,3,3,4),(26.4423043696954,
27.3041253046706,28.2792726369803,29.25441996929,30.2295673015996,31.2047146339093,
32.179861966219),.UNSPECIFIED.);
#503=B_SPLINE_CURVE_WITH_KNOTS('',3,(#20617,#20618,#20619,#20620,#20621,
#20622,#20623,#20624,#20625,#20626,#20627,#20628,#20629,#20630,#20631,#20632,
#20633,#20634,#20635,#20636,#20637,#20638),.UNSPECIFIED.,.F.,.F.,(4,3,3,
3,3,3,3,4),(-28.9853432330879,-28.2792726369803,-27.3041253046706,-26.3289779723609,
-25.3538306400513,-24.3786833077416,-23.403535975432,-22.7021579259084),
 .UNSPECIFIED.);
#504=B_SPLINE_CURVE_WITH_KNOTS('',3,(#20643,#20644,#20645,#20646,#20647,
#20648,#20649,#20650,#20651,#20652,#20653,#20654,#20655,#20656,#20657,#20658,
#20659,#20660,#20661,#20662,#20663,#20664,#20665,#20666,#20667),
 .UNSPECIFIED.,.F.,.F.,(4,3,3,3,3,3,3,3,4),(20.1591190625159,20.478093978503,
21.4532413108126,22.4283886431223,23.403535975432,24.3786833077416,25.3538306400513,
26.328977972361,26.4423043696954),.UNSPECIFIED.);
#505=B_SPLINE_CURVE_WITH_KNOTS('',3,(#20668,#20669,#20670,#20671,#20672,
#20673,#20674,#20675,#20676,#20677,#20678,#20679,#20680,#20681,#20682,#20683,
#20684,#20685,#20686,#20687,#20688,#20689,#20690,#20691,#20692),
 .UNSPECIFIED.,.F.,.F.,(4,3,3,3,3,3,3,3,4),(-22.7021579259084,-22.4283886431223,
-21.4532413108126,-20.478093978503,-19.5029466461933,-18.5277993138836,
-17.552651981574,-16.5775046492643,-16.4189726187288),.UNSPECIFIED.);
#506=B_SPLINE_CURVE_WITH_KNOTS('',3,(#20697,#20698,#20699,#20700,#20701,
#20702,#20703,#20704,#20705,#20706,#20707,#20708,#20709,#20710,#20711,#20712,
#20713,#20714,#20715,#20716,#20717,#20718),.UNSPECIFIED.,.F.,.F.,(4,3,3,
3,3,3,3,4),(13.8759337553363,14.627209984645,15.6023573169546,16.5775046492643,
17.552651981574,18.5277993138836,19.5029466461933,20.1591190625159),
 .UNSPECIFIED.);
#507=B_SPLINE_CURVE_WITH_KNOTS('',3,(#20719,#20720,#20721,#20722,#20723,
#20724,#20725,#20726,#20727,#20728,#20729,#20730,#20731,#20732,#20733,#20734,
#20735,#20736,#20737,#20738,#20739,#20740),.UNSPECIFIED.,.F.,.F.,(4,3,3,
3,3,3,3,4),(-16.4189726187288,-15.6023573169546,-14.627209984645,-13.6520626523353,
-12.6769153200256,-11.701767987716,-10.7266206554063,-10.1357873115492),
 .UNSPECIFIED.);
#508=B_SPLINE_CURVE_WITH_KNOTS('',3,(#20746,#20747,#20748,#20749,#20750,
#20751,#20752,#20753,#20754,#20755,#20756,#20757,#20758),.UNSPECIFIED.,
 .F.,.F.,(4,3,3,3,4),(-3.8526020043696,-2.92544199692899,-1.95029466461933,
-0.975147332309664,0.),.UNSPECIFIED.);
#509=B_SPLINE_CURVE_WITH_KNOTS('',3,(#20761,#20762,#20763,#20764,#20765,
#20766,#20767,#20768,#20769,#20770,#20771,#20772,#20773,#20774,#20775,#20776,
#20777,#20778,#20779),.UNSPECIFIED.,.F.,.F.,(4,3,3,3,3,3,4),(2.02057249175693,
2.925441996929,3.90058932923866,4.87573666154832,5.85088399385799,6.82603132616766,
7.59274844815668),.UNSPECIFIED.);
#510=B_SPLINE_CURVE_WITH_KNOTS('',3,(#20785,#20786,#20787,#20788,#20789,
#20790,#20791),.UNSPECIFIED.,.F.,.F.,(4,1,1,1,4),(40.8407044966673,41.1097812328693,
42.084928565179,43.0600758974886,44.0352232297983),.UNSPECIFIED.);
#511=B_SPLINE_CURVE_WITH_KNOTS('',3,(#20794,#20795,#20796,#20797,#20798,
#20799,#20800),.UNSPECIFIED.,.F.,.F.,(4,1,1,1,4),(40.8407044966673,41.7025254316425,
42.6776727639522,43.6528200962618,44.5576896014339),.UNSPECIFIED.);
#512=B_SPLINE_CURVE_WITH_KNOTS('',3,(#20805,#20806,#20807,#20808,#20809,
#20810,#20811,#20812,#20813,#20814),.UNSPECIFIED.,.F.,.F.,(4,1,1,1,1,1,
1,4),(34.5575191894877,35.2588972390113,36.234044571321,37.2091919036307,
38.1843392359403,39.15948656825,40.1346339005596,40.8407044966673),
 .UNSPECIFIED.);
#513=B_SPLINE_CURVE_WITH_KNOTS('',3,(#20815,#20816,#20817,#20818,#20819,
#20820,#20821,#20822,#20823,#20824,#20825),.UNSPECIFIED.,.F.,.F.,(4,1,1,
1,1,1,1,1,4),(34.5575191894877,34.8764941054748,35.8516414377845,36.8267887700942,
37.8019361024038,38.7770834347135,39.7522307670232,40.7273780993328,40.8407044966673),
 .UNSPECIFIED.);
#514=B_SPLINE_CURVE_WITH_KNOTS('',3,(#20830,#20831,#20832,#20833,#20834,
#20835,#20836,#20837,#20838,#20839,#20840),.UNSPECIFIED.,.F.,.F.,(4,1,1,
1,1,1,1,1,4),(28.2743338823081,28.4328659128437,29.4080132451533,30.383160577463,
31.3583079097727,32.3334552420823,33.308602574392,34.2837499067017,34.5575191894877),
 .UNSPECIFIED.);
#515=B_SPLINE_CURVE_WITH_KNOTS('',3,(#20841,#20842,#20843,#20844,#20845,
#20846,#20847,#20848,#20849,#20850),.UNSPECIFIED.,.F.,.F.,(4,1,1,1,1,1,
1,4),(28.2743338823081,29.0256101116168,30.0007574439265,30.9759047762362,
31.9510521085458,32.9261994408555,33.9013467731652,34.5575191894877),
 .UNSPECIFIED.);
#516=B_SPLINE_CURVE_WITH_KNOTS('',3,(#20855,#20856,#20857,#20858,#20859,
#20860,#20861,#20862,#20863,#20864),.UNSPECIFIED.,.F.,.F.,(4,1,1,1,1,1,
1,4),(21.9911485751285,22.5819819189857,23.5571292512954,24.532276583605,
25.5074239159147,26.4825712482243,27.457718580534,28.2743338823081),
 .UNSPECIFIED.);
#517=B_SPLINE_CURVE_WITH_KNOTS('',3,(#20865,#20866,#20867,#20868,#20869,
#20870,#20871,#20872,#20873,#20874,#20875),.UNSPECIFIED.,.F.,.F.,(4,1,1,
1,1,1,1,1,4),(21.9911485751285,22.1995787854492,23.1747261177589,24.1498734500685,
25.1250207823782,26.1001681146879,27.0753154469975,28.0504627793072,28.2743338823081),
 .UNSPECIFIED.);
#518=B_SPLINE_CURVE_WITH_KNOTS('',3,(#20881,#20882,#20883,#20884,#20885),
 .UNSPECIFIED.,.F.,.F.,(4,1,4),(14.3984001269719,15.3735474592815,15.7079632679489),
 .UNSPECIFIED.);
#519=B_SPLINE_CURVE_WITH_KNOTS('',3,(#20888,#20889,#20890,#20891,#20892),
 .UNSPECIFIED.,.F.,.F.,(4,1,4),(13.8759337553363,14.7808032605084,15.7079632679489),
 .UNSPECIFIED.);
#520=B_SPLINE_CURVE_WITH_KNOTS('',3,(#20894,#20895,#20896,#20897,#20898,
#20899,#20900,#20901,#20902,#20903,#20904),.UNSPECIFIED.,.F.,.F.,(4,1,1,
1,1,1,1,1,4),(15.7079632679489,15.755950592818,16.7310979251277,17.7062452574374,
18.681392589747,19.6565399220567,20.6316872543664,21.606834586676,21.9911485751285),
 .UNSPECIFIED.);
#521=B_SPLINE_CURVE_WITH_KNOTS('',3,(#20905,#20906,#20907,#20908,#20909,
#20910,#20911,#20912,#20913,#20914),.UNSPECIFIED.,.F.,.F.,(4,1,1,1,1,1,
1,4),(15.7079632679489,16.3486947915912,17.3238421239009,18.2989894562105,
19.2741367885202,20.2492841208299,21.2244314531395,21.9911485751285),
 .UNSPECIFIED.);
#522=B_SPLINE_CURVE_WITH_KNOTS('',3,(#21059,#21060,#21061,#21062,#21063,
#21064,#21065,#21066,#21067,#21068,#21069,#21070,#21071,#21072,#21073,#21074,
#21075,#21076,#21077,#21078,#21079,#21080,#21081,#21082,#21083,#21084,#21085,
#21086,#21087,#21088,#21089,#21090,#21091,#21092,#21093,#21094,#21095,#21096,
#21097,#21098,#21099,#21100,#21101,#21102,#21103,#21104,#21105,#21106,#21107),
 .UNSPECIFIED.,.F.,.F.,(4,3,3,3,3,3,3,3,3,3,3,3,3,3,3,3,4),(0.,0.0320333804888866,
0.0505515708593653,0.0603413132804416,0.0917900141854983,0.108096115778005,
0.122914675479851,0.145143248337739,0.168151513577436,0.177516949333476,
0.202471322707608,0.21794283081622,0.231200110368267,0.247503117401854,
0.263651632124391,0.277334442830003,0.286347380332244),.UNSPECIFIED.);
#523=B_SPLINE_CURVE_WITH_KNOTS('',3,(#21108,#21109,#21110,#21111,#21112,
#21113,#21114,#21115,#21116,#21117,#21118,#21119,#21120,#21121,#21122,#21123,
#21124,#21125,#21126,#21127,#21128,#21129,#21130,#21131,#21132,#21133,#21134,
#21135,#21136,#21137,#21138,#21139,#21140,#21141,#21142,#21143,#21144,#21145,
#21146,#21147,#21148,#21149,#21150,#21151,#21152,#21153,#21154,#21155,#21156),
 .UNSPECIFIED.,.F.,.F.,(4,3,3,3,3,3,3,3,3,3,3,3,3,3,3,3,4),(0.,0.0274305464075637,
0.0492901149097146,0.0591933555873536,0.0887250095166089,0.100015570674795,
0.108381796308415,0.130826479038955,0.152531076563578,0.162815893631175,
0.190691958353668,0.212372986031639,0.222945305605857,0.245534254906135,
0.257847836118801,0.274320152521146,0.28514280399515),.UNSPECIFIED.);
#524=B_SPLINE_CURVE_WITH_KNOTS('',3,(#21157,#21158,#21159,#21160,#21161,
#21162,#21163,#21164,#21165,#21166,#21167,#21168,#21169,#21170,#21171,#21172,
#21173,#21174,#21175,#21176,#21177,#21178,#21179,#21180,#21181),
 .UNSPECIFIED.,.F.,.F.,(4,3,3,3,3,3,3,3,4),(-10.1357873115492,-9.75147332309665,
-8.77632599078699,-7.80117865847732,-6.82603132616766,-5.85088399385799,
-4.87573666154833,-3.90058932923866,-3.8526020043696),.UNSPECIFIED.);
#525=B_SPLINE_CURVE_WITH_KNOTS('',3,(#21326,#21327,#21328,#21329,#21330,
#21331,#21332,#21333,#21334,#21335,#21336,#21337,#21338,#21339,#21340,#21341,
#21342,#21343,#21344,#21345,#21346,#21347,#21348,#21349,#21350,#21351,#21352,
#21353,#21354,#21355,#21356,#21357,#21358,#21359,#21360,#21361,#21362,#21363,
#21364,#21365,#21366,#21367,#21368,#21369,#21370,#21371,#21372,#21373,#21374),
 .UNSPECIFIED.,.F.,.F.,(4,3,3,3,3,3,3,3,3,3,3,3,3,3,3,3,4),(0.,0.0274305890506951,
0.0492901290331875,0.0591933603491513,0.0887250177779717,0.100015607166709,
0.108381835831352,0.13082647903896,0.152531071764912,0.162815892251191,
0.190691957318683,0.212372984486691,0.22294529735758,0.245534140364172,
0.257847701250626,0.274320152521159,0.285142803995162),.UNSPECIFIED.);
#526=B_SPLINE_CURVE_WITH_KNOTS('',3,(#21375,#21376,#21377,#21378,#21379,
#21380,#21381,#21382,#21383,#21384,#21385,#21386,#21387,#21388,#21389,#21390,
#21391,#21392,#21393,#21394,#21395,#21396,#21397,#21398,#21399),
 .UNSPECIFIED.,.F.,.F.,(4,3,3,3,3,3,3,3,4),(7.59274844815668,7.80117865847732,
8.77632599078698,9.75147332309665,10.7266206554063,11.701767987716,12.6769153200256,
13.6520626523353,13.8759337553363),.UNSPECIFIED.);
#527=B_SPLINE_CURVE_WITH_KNOTS('',3,(#21400,#21401,#21402,#21403,#21404,
#21405,#21406,#21407,#21408,#21409,#21410,#21411,#21412,#21413,#21414,#21415,
#21416,#21417,#21418,#21419,#21420,#21421,#21422,#21423,#21424,#21425,#21426,
#21427,#21428,#21429,#21430,#21431,#21432,#21433,#21434,#21435,#21436,#21437,
#21438,#21439,#21440,#21441,#21442,#21443,#21444,#21445,#21446,#21447,#21448),
 .UNSPECIFIED.,.F.,.F.,(4,3,3,3,3,3,3,3,3,3,3,3,3,3,3,3,4),(0.,0.0320334058164849,
0.0505515938322513,0.0603413311462071,0.0917900214840119,0.108096111687201,
0.122914678304232,0.145143248337743,0.168151527562726,0.177516955081398,
0.202471327018552,0.217942288122009,0.231200024743484,0.24750284136614,
0.263651600306541,0.277334442830014,0.286347380332252),.UNSPECIFIED.);
#528=B_SPLINE_CURVE_WITH_KNOTS('',3,(#21586,#21587,#21588,#21589,#21590),
 .UNSPECIFIED.,.F.,.F.,(4,1,4),(-0.105712226943305,-0.0453052401185593,
0.),.UNSPECIFIED.);
#529=B_SPLINE_CURVE_WITH_KNOTS('',3,(#21593,#21594,#21595,#21596,#21597),
 .UNSPECIFIED.,.F.,.F.,(4,1,4),(0.,0.0453052401185593,0.105712226943305),
 .UNSPECIFIED.);
#530=B_SPLINE_CURVE_WITH_KNOTS('',3,(#21632,#21633,#21634,#21635,#21636),
 .UNSPECIFIED.,.F.,.F.,(4,1,4),(-0.105712227002476,-0.0453052401439183,
0.),.UNSPECIFIED.);
#531=B_SPLINE_CURVE_WITH_KNOTS('',3,(#21637,#21638,#21639,#21640,#21641),
 .UNSPECIFIED.,.F.,.F.,(4,1,4),(0.,0.0453052401439183,0.105712227002476),
 .UNSPECIFIED.);
#532=B_SPLINE_CURVE_WITH_KNOTS('',3,(#21670,#21671,#21672,#21673,#21674),
 .UNSPECIFIED.,.F.,.F.,(4,1,4),(-9.8118987320379,-4.20509945658767,0.),
 .UNSPECIFIED.);
#533=B_SPLINE_CURVE_WITH_KNOTS('',3,(#21675,#21676,#21677,#21678,#21679),
 .UNSPECIFIED.,.F.,.F.,(4,1,4),(0.,4.20509945658767,9.8118987320379),
 .UNSPECIFIED.);
#534=B_SPLINE_CURVE_WITH_KNOTS('',3,(#21708,#21709,#21710,#21711,#21712),
 .UNSPECIFIED.,.F.,.F.,(4,1,4),(-0.103805833027027,-0.0444882141544403,
0.),.UNSPECIFIED.);
#535=B_SPLINE_CURVE_WITH_KNOTS('',3,(#21713,#21714,#21715,#21716,#21717),
 .UNSPECIFIED.,.F.,.F.,(4,1,4),(0.,0.0444882141544403,0.103805833027027),
 .UNSPECIFIED.);
#536=B_SPLINE_CURVE_WITH_KNOTS('',3,(#21752,#21753,#21754,#21755,#21756),
 .UNSPECIFIED.,.F.,.F.,(4,1,4),(-0.103805833117318,-0.0444882141931362,
-2.06005858395869E-18),.UNSPECIFIED.);
#537=B_SPLINE_CURVE_WITH_KNOTS('',3,(#21757,#21758,#21759,#21760,#21761),
 .UNSPECIFIED.,.F.,.F.,(4,1,4),(2.06005858395869E-18,0.0444882141931362,
0.103805833117318),.UNSPECIFIED.);
#538=B_SPLINE_CURVE_WITH_KNOTS('',3,(#21787,#21788,#21789,#21790,#21791),
 .UNSPECIFIED.,.F.,.F.,(4,1,4),(-9.81189789495051,-4.20509909783593,0.),
 .UNSPECIFIED.);
#539=B_SPLINE_CURVE_WITH_KNOTS('',3,(#21792,#21793,#21794,#21795,#21796),
 .UNSPECIFIED.,.F.,.F.,(4,1,4),(0.,4.20509909783593,9.81189789495051),
 .UNSPECIFIED.);
#540=B_SPLINE_CURVE_WITH_KNOTS('',3,(#21799,#21800,#21801,#21802),
 .UNSPECIFIED.,.F.,.F.,(4,4),(0.00062434729305816,0.125151053668407),
 .UNSPECIFIED.);
#541=B_SPLINE_CURVE_WITH_KNOTS('',3,(#21805,#21806,#21807,#21808),
 .UNSPECIFIED.,.F.,.F.,(4,4),(-0.125151053668407,-0.000624347293058304),
 .UNSPECIFIED.);
#542=B_SPLINE_CURVE_WITH_KNOTS('',3,(#21830,#21831,#21832,#21833),
 .UNSPECIFIED.,.F.,.F.,(4,4),(-0.124859357077656,3.91613824701764E-16),
 .UNSPECIFIED.);
#543=B_SPLINE_CURVE_WITH_KNOTS('',3,(#21834,#21835,#21836,#21837,#21838,
#21839,#21840,#21841,#21842,#21843,#21844,#21845,#21846,#21847,#21848,#21849,
#21850,#21851,#21852,#21853,#21854,#21855,#21856,#21857,#21858,#21859,#21860,
#21861),.UNSPECIFIED.,.F.,.F.,(4,3,3,3,3,3,3,3,3,4),(0.,0.032270992282214,
0.0586131010579366,0.0908535483049998,0.095660418056781,0.117090121226367,
0.149479430319939,0.17008966569926,0.202270498561131,0.223122165115773),
 .UNSPECIFIED.);
#544=B_SPLINE_CURVE_WITH_KNOTS('',3,(#21879,#21880,#21881,#21882),
 .UNSPECIFIED.,.F.,.F.,(4,4),(1.57426155444895E-16,0.124757292074316),
 .UNSPECIFIED.);
#545=B_SPLINE_CURVE_WITH_KNOTS('',3,(#21883,#21884,#21885,#21886),
 .UNSPECIFIED.,.F.,.F.,(4,4),(0.0135518988075539,0.986045335056425),
 .UNSPECIFIED.);
#546=B_SPLINE_CURVE_WITH_KNOTS('',3,(#21908,#21909,#21910,#21911),
 .UNSPECIFIED.,.F.,.F.,(4,4),(-0.124959300034279,-0.000432357919845506),
 .UNSPECIFIED.);
#547=B_SPLINE_CURVE_WITH_KNOTS('',3,(#21912,#21913,#21914,#21915,#21916,
#21917,#21918,#21919,#21920,#21921,#21922,#21923,#21924,#21925,#21926,#21927,
#21928,#21929,#21930,#21931,#21932,#21933,#21934,#21935,#21936,#21937,#21938,
#21939),.UNSPECIFIED.,.F.,.F.,(4,3,3,3,3,3,3,3,3,4),(0.,0.0322720371751271,
0.0586511315716134,0.0908889384397039,0.0974306796249642,0.117149930269381,
0.149553095257184,0.172178760978465,0.204364325027201,0.227238249760569),
 .UNSPECIFIED.);
#548=B_SPLINE_CURVE_WITH_KNOTS('',3,(#21943,#21944,#21945,#21946),
 .UNSPECIFIED.,.F.,.F.,(4,4),(0.000432357919845864,0.12495930003428),
 .UNSPECIFIED.);
#549=B_SPLINE_CURVE_WITH_KNOTS('',3,(#21969,#21970,#21971,#21972,#21973,
#21974,#21975,#21976,#21977,#21978,#21979,#21980,#21981,#21982,#21983,#21984,
#21985,#21986,#21987,#21988,#21989,#21990,#21991,#21992,#21993,#21994,#21995,
#21996),.UNSPECIFIED.,.F.,.F.,(4,3,3,3,3,3,3,3,3,4),(0.,0.0322770007607463,
0.0586509099358757,0.0908890592373503,0.0956758252683957,0.117149647541228,
0.149540928065794,0.17012301918783,0.202296660223156,0.2231241621482),
 .UNSPECIFIED.);
#550=B_SPLINE_CURVE_WITH_KNOTS('',3,(#21997,#21998,#21999,#22000),
 .UNSPECIFIED.,.F.,.F.,(4,4),(1.94722710178397E-16,0.124859357077656),
 .UNSPECIFIED.);
#551=B_SPLINE_CURVE_WITH_KNOTS('',3,(#22022,#22023,#22024,#22025),
 .UNSPECIFIED.,.F.,.F.,(4,4),(-0.124757292074297,-2.43294967505747E-16),
 .UNSPECIFIED.);
#552=B_SPLINE_CURVE_WITH_KNOTS('',3,(#22026,#22027,#22028,#22029,#22030,
#22031,#22032,#22033,#22034,#22035,#22036,#22037,#22038,#22039,#22040,#22041,
#22042,#22043,#22044,#22045,#22046,#22047,#22048,#22049,#22050,#22051,#22052,
#22053),.UNSPECIFIED.,.F.,.F.,(4,3,3,3,3,3,3,3,3,4),(0.,0.0322677829554273,
0.0586251784806003,0.0908644978360158,0.097419835848357,0.117108565494702,
0.149510109206483,0.172155480916619,0.204345933772222,0.227236831322489),
 .UNSPECIFIED.);
#553=B_SPLINE_CURVE_WITH_KNOTS('',3,(#22055,#22056,#22057,#22058),
 .UNSPECIFIED.,.F.,.F.,(4,4),(0.0139546649435756,0.986448101192446),
 .UNSPECIFIED.);
#554=SHAPE_REPRESENTATION_RELATIONSHIP('SRR','None',#22173,#563);
#555=SHAPE_REPRESENTATION_RELATIONSHIP('SRR','None',#22174,#564);
#556=SHAPE_REPRESENTATION_RELATIONSHIP('SRR','None',#22175,#565);
#557=SHAPE_REPRESENTATION_RELATIONSHIP('SRR','None',#22177,#566);
#558=SHAPE_REPRESENTATION_RELATIONSHIP('SRR','None',#22178,#567);
#559=SHAPE_REPRESENTATION_RELATIONSHIP('SRR','None',#22179,#568);
#560=SHAPE_REPRESENTATION_RELATIONSHIP('SRR','None',#22180,#569);
#561=SHAPE_REPRESENTATION_RELATIONSHIP('SRR','None',#22181,#570);
#562=SHAPE_REPRESENTATION_RELATIONSHIP('SRR','None',#22182,#571);
#563=ADVANCED_BREP_SHAPE_REPRESENTATION('',(#581),#22119);
#564=ADVANCED_BREP_SHAPE_REPRESENTATION('',(#582),#22120);
#565=ADVANCED_BREP_SHAPE_REPRESENTATION('',(#583),#22121);
#566=ADVANCED_BREP_SHAPE_REPRESENTATION('',(#584),#22123);
#567=ADVANCED_BREP_SHAPE_REPRESENTATION('',(#585),#22124);
#568=ADVANCED_BREP_SHAPE_REPRESENTATION('',(#586),#22125);
#569=ADVANCED_BREP_SHAPE_REPRESENTATION('',(#587),#22126);
#570=ADVANCED_BREP_SHAPE_REPRESENTATION('',(#588),#22127);
#571=ADVANCED_BREP_SHAPE_REPRESENTATION('',(#589),#22128);
#572=STYLED_ITEM('',(#22232),#581);
#573=STYLED_ITEM('',(#22233),#582);
#574=STYLED_ITEM('',(#22234),#583);
#575=STYLED_ITEM('',(#22235),#584);
#576=STYLED_ITEM('',(#22235),#585);
#577=STYLED_ITEM('',(#22234),#586);
#578=STYLED_ITEM('',(#22236),#587);
#579=STYLED_ITEM('',(#22237),#588);
#580=STYLED_ITEM('',(#22238),#589);
#581=MANIFOLD_SOLID_BREP('Body1',#8803);
#582=MANIFOLD_SOLID_BREP('Body1',#8804);
#583=MANIFOLD_SOLID_BREP('Body1',#8805);
#584=MANIFOLD_SOLID_BREP('Body1',#8806);
#585=MANIFOLD_SOLID_BREP('Body1',#8807);
#586=MANIFOLD_SOLID_BREP('Body1',#8808);
#587=MANIFOLD_SOLID_BREP('Body1',#8809);
#588=MANIFOLD_SOLID_BREP('Body1',#8810);
#589=MANIFOLD_SOLID_BREP('Body1',#8811);
#590=FACE_BOUND('',#1511,.T.);
#591=FACE_BOUND('',#1512,.T.);
#592=FACE_BOUND('',#1513,.T.);
#593=FACE_BOUND('',#1522,.T.);
#594=FACE_BOUND('',#1523,.T.);
#595=FACE_BOUND('',#1524,.T.);
#596=FACE_BOUND('',#1528,.T.);
#597=FACE_BOUND('',#1530,.T.);
#598=FACE_BOUND('',#1533,.T.);
#599=FACE_BOUND('',#1551,.T.);
#600=FACE_BOUND('',#1552,.T.);
#601=FACE_BOUND('',#1553,.T.);
#602=FACE_BOUND('',#1560,.T.);
#603=FACE_BOUND('',#1563,.T.);
#604=FACE_BOUND('',#1574,.T.);
#605=FACE_BOUND('',#1576,.T.);
#606=FACE_BOUND('',#1588,.T.);
#607=FACE_BOUND('',#1609,.T.);
#608=FACE_BOUND('',#1610,.T.);
#609=FACE_BOUND('',#1611,.T.);
#610=FACE_BOUND('',#1646,.T.);
#611=FACE_BOUND('',#1647,.T.);
#612=FACE_BOUND('',#1648,.T.);
#613=FACE_BOUND('',#1649,.T.);
#614=FACE_BOUND('',#1650,.T.);
#615=FACE_BOUND('',#1651,.T.);
#616=FACE_BOUND('',#1661,.T.);
#617=FACE_BOUND('',#1662,.T.);
#618=FACE_BOUND('',#1663,.T.);
#619=FACE_BOUND('',#1671,.T.);
#620=FACE_BOUND('',#1679,.T.);
#621=FACE_BOUND('',#1694,.T.);
#622=FACE_BOUND('',#1696,.T.);
#623=FACE_BOUND('',#1708,.T.);
#624=FACE_BOUND('',#1729,.T.);
#625=FACE_BOUND('',#1730,.T.);
#626=FACE_BOUND('',#1731,.T.);
#627=FACE_BOUND('',#1766,.T.);
#628=FACE_BOUND('',#1767,.T.);
#629=FACE_BOUND('',#1768,.T.);
#630=FACE_BOUND('',#1769,.T.);
#631=FACE_BOUND('',#1770,.T.);
#632=FACE_BOUND('',#1771,.T.);
#633=FACE_BOUND('',#1847,.T.);
#634=FACE_BOUND('',#1850,.T.);
#635=FACE_BOUND('',#1866,.T.);
#636=FACE_BOUND('',#1875,.T.);
#637=FACE_BOUND('',#1879,.T.);
#638=FACE_BOUND('',#1883,.T.);
#639=FACE_BOUND('',#1887,.T.);
#640=FACE_BOUND('',#1891,.T.);
#641=FACE_BOUND('',#1911,.T.);
#642=FACE_BOUND('',#1912,.T.);
#643=FACE_BOUND('',#1917,.T.);
#644=FACE_BOUND('',#1918,.T.);
#645=FACE_BOUND('',#1919,.T.);
#646=FACE_BOUND('',#1920,.T.);
#647=FACE_BOUND('',#1921,.T.);
#648=FACE_BOUND('',#1922,.T.);
#649=FACE_BOUND('',#1927,.T.);
#650=FACE_BOUND('',#1929,.T.);
#651=PLANE('',#8923);
#652=PLANE('',#8924);
#653=PLANE('',#8925);
#654=PLANE('',#8926);
#655=PLANE('',#8927);
#656=PLANE('',#8928);
#657=PLANE('',#8929);
#658=PLANE('',#8930);
#659=PLANE('',#8931);
#660=PLANE('',#8932);
#661=PLANE('',#8933);
#662=PLANE('',#8934);
#663=PLANE('',#8935);
#664=PLANE('',#8936);
#665=PLANE('',#8937);
#666=PLANE('',#8938);
#667=PLANE('',#8939);
#668=PLANE('',#8940);
#669=PLANE('',#8941);
#670=PLANE('',#8942);
#671=PLANE('',#8943);
#672=PLANE('',#8944);
#673=PLANE('',#8945);
#674=PLANE('',#8946);
#675=PLANE('',#8947);
#676=PLANE('',#8948);
#677=PLANE('',#8949);
#678=PLANE('',#8950);
#679=PLANE('',#8951);
#680=PLANE('',#8952);
#681=PLANE('',#8953);
#682=PLANE('',#8954);
#683=PLANE('',#8955);
#684=PLANE('',#8956);
#685=PLANE('',#8957);
#686=PLANE('',#8958);
#687=PLANE('',#8959);
#688=PLANE('',#8960);
#689=PLANE('',#8961);
#690=PLANE('',#8962);
#691=PLANE('',#8963);
#692=PLANE('',#8964);
#693=PLANE('',#8965);
#694=PLANE('',#8966);
#695=PLANE('',#8967);
#696=PLANE('',#8968);
#697=PLANE('',#8969);
#698=PLANE('',#8970);
#699=PLANE('',#8971);
#700=PLANE('',#8972);
#701=PLANE('',#8973);
#702=PLANE('',#8974);
#703=PLANE('',#8975);
#704=PLANE('',#8976);
#705=PLANE('',#8977);
#706=PLANE('',#8978);
#707=PLANE('',#8979);
#708=PLANE('',#8980);
#709=PLANE('',#8981);
#710=PLANE('',#8982);
#711=PLANE('',#8983);
#712=PLANE('',#8984);
#713=PLANE('',#8985);
#714=PLANE('',#8986);
#715=PLANE('',#8987);
#716=PLANE('',#8988);
#717=PLANE('',#8989);
#718=PLANE('',#8990);
#719=PLANE('',#8991);
#720=PLANE('',#8992);
#721=PLANE('',#8993);
#722=PLANE('',#8994);
#723=PLANE('',#8995);
#724=PLANE('',#8996);
#725=PLANE('',#8997);
#726=PLANE('',#8998);
#727=PLANE('',#8999);
#728=PLANE('',#9000);
#729=PLANE('',#9001);
#730=PLANE('',#9002);
#731=PLANE('',#9003);
#732=PLANE('',#9004);
#733=PLANE('',#9005);
#734=PLANE('',#9006);
#735=PLANE('',#9007);
#736=PLANE('',#9008);
#737=PLANE('',#9009);
#738=PLANE('',#9010);
#739=PLANE('',#9011);
#740=PLANE('',#9012);
#741=PLANE('',#9013);
#742=PLANE('',#9014);
#743=PLANE('',#9015);
#744=PLANE('',#9016);
#745=PLANE('',#9017);
#746=PLANE('',#9018);
#747=PLANE('',#9019);
#748=PLANE('',#9020);
#749=PLANE('',#9021);
#750=PLANE('',#9022);
#751=PLANE('',#9023);
#752=PLANE('',#9024);
#753=PLANE('',#9025);
#754=PLANE('',#9026);
#755=PLANE('',#9027);
#756=PLANE('',#9028);
#757=PLANE('',#9029);
#758=PLANE('',#9030);
#759=PLANE('',#9031);
#760=PLANE('',#9032);
#761=PLANE('',#9033);
#762=PLANE('',#9034);
#763=PLANE('',#9035);
#764=PLANE('',#9036);
#765=PLANE('',#9037);
#766=PLANE('',#9038);
#767=PLANE('',#9039);
#768=PLANE('',#9040);
#769=PLANE('',#9041);
#770=PLANE('',#9042);
#771=PLANE('',#9043);
#772=PLANE('',#9044);
#773=PLANE('',#9049);
#774=PLANE('',#9050);
#775=PLANE('',#9051);
#776=PLANE('',#9052);
#777=PLANE('',#9053);
#778=PLANE('',#9054);
#779=PLANE('',#9055);
#780=PLANE('',#9062);
#781=PLANE('',#9064);
#782=PLANE('',#9068);
#783=PLANE('',#9073);
#784=PLANE('',#9075);
#785=PLANE('',#9077);
#786=PLANE('',#9078);
#787=PLANE('',#9079);
#788=PLANE('',#9086);
#789=PLANE('',#9097);
#790=PLANE('',#9114);
#791=PLANE('',#9119);
#792=PLANE('',#9125);
#793=PLANE('',#9126);
#794=PLANE('',#9127);
#795=PLANE('',#9128);
#796=PLANE('',#9129);
#797=PLANE('',#9130);
#798=PLANE('',#9131);
#799=PLANE('',#9132);
#800=PLANE('',#9134);
#801=PLANE('',#9136);
#802=PLANE('',#9137);
#803=PLANE('',#9138);
#804=PLANE('',#9139);
#805=PLANE('',#9140);
#806=PLANE('',#9141);
#807=PLANE('',#9142);
#808=PLANE('',#9143);
#809=PLANE('',#9144);
#810=PLANE('',#9145);
#811=PLANE('',#9146);
#812=PLANE('',#9150);
#813=PLANE('',#9152);
#814=PLANE('',#9153);
#815=PLANE('',#9154);
#816=PLANE('',#9155);
#817=PLANE('',#9156);
#818=PLANE('',#9157);
#819=PLANE('',#9159);
#820=PLANE('',#9176);
#821=PLANE('',#9195);
#822=PLANE('',#9196);
#823=PLANE('',#9197);
#824=PLANE('',#9207);
#825=PLANE('',#9211);
#826=PLANE('',#9212);
#827=PLANE('',#9213);
#828=PLANE('',#9214);
#829=PLANE('',#9215);
#830=PLANE('',#9216);
#831=PLANE('',#9217);
#832=PLANE('',#9219);
#833=PLANE('',#9220);
#834=PLANE('',#9221);
#835=PLANE('',#9222);
#836=PLANE('',#9223);
#837=PLANE('',#9224);
#838=PLANE('',#9225);
#839=PLANE('',#9241);
#840=PLANE('',#9242);
#841=PLANE('',#9243);
#842=PLANE('',#9244);
#843=PLANE('',#9245);
#844=PLANE('',#9246);
#845=PLANE('',#9247);
#846=PLANE('',#9248);
#847=PLANE('',#9250);
#848=PLANE('',#9252);
#849=PLANE('',#9253);
#850=PLANE('',#9254);
#851=PLANE('',#9255);
#852=PLANE('',#9256);
#853=PLANE('',#9257);
#854=PLANE('',#9258);
#855=PLANE('',#9259);
#856=PLANE('',#9260);
#857=PLANE('',#9261);
#858=PLANE('',#9262);
#859=PLANE('',#9266);
#860=PLANE('',#9268);
#861=PLANE('',#9269);
#862=PLANE('',#9270);
#863=PLANE('',#9271);
#864=PLANE('',#9272);
#865=PLANE('',#9273);
#866=PLANE('',#9275);
#867=PLANE('',#9292);
#868=PLANE('',#9311);
#869=PLANE('',#9312);
#870=PLANE('',#9313);
#871=PLANE('',#9383);
#872=PLANE('',#9384);
#873=PLANE('',#9385);
#874=PLANE('',#9386);
#875=PLANE('',#9387);
#876=PLANE('',#9388);
#877=PLANE('',#9389);
#878=PLANE('',#9390);
#879=PLANE('',#9394);
#880=PLANE('',#9395);
#881=PLANE('',#9413);
#882=PLANE('',#9415);
#883=PLANE('',#9416);
#884=PLANE('',#9417);
#885=PLANE('',#9418);
#886=PLANE('',#9419);
#887=PLANE('',#9420);
#888=PLANE('',#9421);
#889=PLANE('',#9429);
#890=PLANE('',#9434);
#891=PLANE('',#9435);
#892=PLANE('',#9440);
#893=PLANE('',#9441);
#894=PLANE('',#9446);
#895=PLANE('',#9447);
#896=PLANE('',#9452);
#897=PLANE('',#9471);
#898=PLANE('',#9472);
#899=PLANE('',#9473);
#900=PLANE('',#9474);
#901=PLANE('',#9490);
#902=PLANE('',#9491);
#903=FACE_OUTER_BOUND('',#1386,.T.);
#904=FACE_OUTER_BOUND('',#1387,.T.);
#905=FACE_OUTER_BOUND('',#1388,.T.);
#906=FACE_OUTER_BOUND('',#1389,.T.);
#907=FACE_OUTER_BOUND('',#1390,.T.);
#908=FACE_OUTER_BOUND('',#1391,.T.);
#909=FACE_OUTER_BOUND('',#1392,.T.);
#910=FACE_OUTER_BOUND('',#1393,.T.);
#911=FACE_OUTER_BOUND('',#1394,.T.);
#912=FACE_OUTER_BOUND('',#1395,.T.);
#913=FACE_OUTER_BOUND('',#1396,.T.);
#914=FACE_OUTER_BOUND('',#1397,.T.);
#915=FACE_OUTER_BOUND('',#1398,.T.);
#916=FACE_OUTER_BOUND('',#1399,.T.);
#917=FACE_OUTER_BOUND('',#1400,.T.);
#918=FACE_OUTER_BOUND('',#1401,.T.);
#919=FACE_OUTER_BOUND('',#1402,.T.);
#920=FACE_OUTER_BOUND('',#1403,.T.);
#921=FACE_OUTER_BOUND('',#1404,.T.);
#922=FACE_OUTER_BOUND('',#1405,.T.);
#923=FACE_OUTER_BOUND('',#1406,.T.);
#924=FACE_OUTER_BOUND('',#1407,.T.);
#925=FACE_OUTER_BOUND('',#1408,.T.);
#926=FACE_OUTER_BOUND('',#1409,.T.);
#927=FACE_OUTER_BOUND('',#1410,.T.);
#928=FACE_OUTER_BOUND('',#1411,.T.);
#929=FACE_OUTER_BOUND('',#1412,.T.);
#930=FACE_OUTER_BOUND('',#1413,.T.);
#931=FACE_OUTER_BOUND('',#1414,.T.);
#932=FACE_OUTER_BOUND('',#1415,.T.);
#933=FACE_OUTER_BOUND('',#1416,.T.);
#934=FACE_OUTER_BOUND('',#1417,.T.);
#935=FACE_OUTER_BOUND('',#1418,.T.);
#936=FACE_OUTER_BOUND('',#1419,.T.);
#937=FACE_OUTER_BOUND('',#1420,.T.);
#938=FACE_OUTER_BOUND('',#1421,.T.);
#939=FACE_OUTER_BOUND('',#1422,.T.);
#940=FACE_OUTER_BOUND('',#1423,.T.);
#941=FACE_OUTER_BOUND('',#1424,.T.);
#942=FACE_OUTER_BOUND('',#1425,.T.);
#943=FACE_OUTER_BOUND('',#1426,.T.);
#944=FACE_OUTER_BOUND('',#1427,.T.);
#945=FACE_OUTER_BOUND('',#1428,.T.);
#946=FACE_OUTER_BOUND('',#1429,.T.);
#947=FACE_OUTER_BOUND('',#1430,.T.);
#948=FACE_OUTER_BOUND('',#1431,.T.);
#949=FACE_OUTER_BOUND('',#1432,.T.);
#950=FACE_OUTER_BOUND('',#1433,.T.);
#951=FACE_OUTER_BOUND('',#1434,.T.);
#952=FACE_OUTER_BOUND('',#1435,.T.);
#953=FACE_OUTER_BOUND('',#1436,.T.);
#954=FACE_OUTER_BOUND('',#1437,.T.);
#955=FACE_OUTER_BOUND('',#1438,.T.);
#956=FACE_OUTER_BOUND('',#1439,.T.);
#957=FACE_OUTER_BOUND('',#1440,.T.);
#958=FACE_OUTER_BOUND('',#1441,.T.);
#959=FACE_OUTER_BOUND('',#1442,.T.);
#960=FACE_OUTER_BOUND('',#1443,.T.);
#961=FACE_OUTER_BOUND('',#1444,.T.);
#962=FACE_OUTER_BOUND('',#1445,.T.);
#963=FACE_OUTER_BOUND('',#1446,.T.);
#964=FACE_OUTER_BOUND('',#1447,.T.);
#965=FACE_OUTER_BOUND('',#1448,.T.);
#966=FACE_OUTER_BOUND('',#1449,.T.);
#967=FACE_OUTER_BOUND('',#1450,.T.);
#968=FACE_OUTER_BOUND('',#1451,.T.);
#969=FACE_OUTER_BOUND('',#1452,.T.);
#970=FACE_OUTER_BOUND('',#1453,.T.);
#971=FACE_OUTER_BOUND('',#1454,.T.);
#972=FACE_OUTER_BOUND('',#1455,.T.);
#973=FACE_OUTER_BOUND('',#1456,.T.);
#974=FACE_OUTER_BOUND('',#1457,.T.);
#975=FACE_OUTER_BOUND('',#1458,.T.);
#976=FACE_OUTER_BOUND('',#1459,.T.);
#977=FACE_OUTER_BOUND('',#1460,.T.);
#978=FACE_OUTER_BOUND('',#1461,.T.);
#979=FACE_OUTER_BOUND('',#1462,.T.);
#980=FACE_OUTER_BOUND('',#1463,.T.);
#981=FACE_OUTER_BOUND('',#1464,.T.);
#982=FACE_OUTER_BOUND('',#1465,.T.);
#983=FACE_OUTER_BOUND('',#1466,.T.);
#984=FACE_OUTER_BOUND('',#1467,.T.);
#985=FACE_OUTER_BOUND('',#1468,.T.);
#986=FACE_OUTER_BOUND('',#1469,.T.);
#987=FACE_OUTER_BOUND('',#1470,.T.);
#988=FACE_OUTER_BOUND('',#1471,.T.);
#989=FACE_OUTER_BOUND('',#1472,.T.);
#990=FACE_OUTER_BOUND('',#1473,.T.);
#991=FACE_OUTER_BOUND('',#1474,.T.);
#992=FACE_OUTER_BOUND('',#1475,.T.);
#993=FACE_OUTER_BOUND('',#1476,.T.);
#994=FACE_OUTER_BOUND('',#1477,.T.);
#995=FACE_OUTER_BOUND('',#1478,.T.);
#996=FACE_OUTER_BOUND('',#1479,.T.);
#997=FACE_OUTER_BOUND('',#1480,.T.);
#998=FACE_OUTER_BOUND('',#1481,.T.);
#999=FACE_OUTER_BOUND('',#1482,.T.);
#1000=FACE_OUTER_BOUND('',#1483,.T.);
#1001=FACE_OUTER_BOUND('',#1484,.T.);
#1002=FACE_OUTER_BOUND('',#1485,.T.);
#1003=FACE_OUTER_BOUND('',#1486,.T.);
#1004=FACE_OUTER_BOUND('',#1487,.T.);
#1005=FACE_OUTER_BOUND('',#1488,.T.);
#1006=FACE_OUTER_BOUND('',#1489,.T.);
#1007=FACE_OUTER_BOUND('',#1490,.T.);
#1008=FACE_OUTER_BOUND('',#1491,.T.);
#1009=FACE_OUTER_BOUND('',#1492,.T.);
#1010=FACE_OUTER_BOUND('',#1493,.T.);
#1011=FACE_OUTER_BOUND('',#1494,.T.);
#1012=FACE_OUTER_BOUND('',#1495,.T.);
#1013=FACE_OUTER_BOUND('',#1496,.T.);
#1014=FACE_OUTER_BOUND('',#1497,.T.);
#1015=FACE_OUTER_BOUND('',#1498,.T.);
#1016=FACE_OUTER_BOUND('',#1499,.T.);
#1017=FACE_OUTER_BOUND('',#1500,.T.);
#1018=FACE_OUTER_BOUND('',#1501,.T.);
#1019=FACE_OUTER_BOUND('',#1502,.T.);
#1020=FACE_OUTER_BOUND('',#1503,.T.);
#1021=FACE_OUTER_BOUND('',#1504,.T.);
#1022=FACE_OUTER_BOUND('',#1505,.T.);
#1023=FACE_OUTER_BOUND('',#1506,.T.);
#1024=FACE_OUTER_BOUND('',#1507,.T.);
#1025=FACE_OUTER_BOUND('',#1508,.T.);
#1026=FACE_OUTER_BOUND('',#1509,.T.);
#1027=FACE_OUTER_BOUND('',#1510,.T.);
#1028=FACE_OUTER_BOUND('',#1514,.T.);
#1029=FACE_OUTER_BOUND('',#1515,.T.);
#1030=FACE_OUTER_BOUND('',#1516,.T.);
#1031=FACE_OUTER_BOUND('',#1517,.T.);
#1032=FACE_OUTER_BOUND('',#1518,.T.);
#1033=FACE_OUTER_BOUND('',#1519,.T.);
#1034=FACE_OUTER_BOUND('',#1520,.T.);
#1035=FACE_OUTER_BOUND('',#1521,.T.);
#1036=FACE_OUTER_BOUND('',#1525,.T.);
#1037=FACE_OUTER_BOUND('',#1526,.T.);
#1038=FACE_OUTER_BOUND('',#1527,.T.);
#1039=FACE_OUTER_BOUND('',#1529,.T.);
#1040=FACE_OUTER_BOUND('',#1531,.T.);
#1041=FACE_OUTER_BOUND('',#1532,.T.);
#1042=FACE_OUTER_BOUND('',#1534,.T.);
#1043=FACE_OUTER_BOUND('',#1535,.T.);
#1044=FACE_OUTER_BOUND('',#1536,.T.);
#1045=FACE_OUTER_BOUND('',#1537,.T.);
#1046=FACE_OUTER_BOUND('',#1538,.T.);
#1047=FACE_OUTER_BOUND('',#1539,.T.);
#1048=FACE_OUTER_BOUND('',#1540,.T.);
#1049=FACE_OUTER_BOUND('',#1541,.T.);
#1050=FACE_OUTER_BOUND('',#1542,.T.);
#1051=FACE_OUTER_BOUND('',#1543,.T.);
#1052=FACE_OUTER_BOUND('',#1544,.T.);
#1053=FACE_OUTER_BOUND('',#1545,.T.);
#1054=FACE_OUTER_BOUND('',#1546,.T.);
#1055=FACE_OUTER_BOUND('',#1547,.T.);
#1056=FACE_OUTER_BOUND('',#1548,.T.);
#1057=FACE_OUTER_BOUND('',#1549,.T.);
#1058=FACE_OUTER_BOUND('',#1550,.T.);
#1059=FACE_OUTER_BOUND('',#1554,.T.);
#1060=FACE_OUTER_BOUND('',#1555,.T.);
#1061=FACE_OUTER_BOUND('',#1556,.T.);
#1062=FACE_OUTER_BOUND('',#1557,.T.);
#1063=FACE_OUTER_BOUND('',#1558,.T.);
#1064=FACE_OUTER_BOUND('',#1559,.T.);
#1065=FACE_OUTER_BOUND('',#1561,.T.);
#1066=FACE_OUTER_BOUND('',#1562,.T.);
#1067=FACE_OUTER_BOUND('',#1564,.T.);
#1068=FACE_OUTER_BOUND('',#1565,.T.);
#1069=FACE_OUTER_BOUND('',#1566,.T.);
#1070=FACE_OUTER_BOUND('',#1567,.T.);
#1071=FACE_OUTER_BOUND('',#1568,.T.);
#1072=FACE_OUTER_BOUND('',#1569,.T.);
#1073=FACE_OUTER_BOUND('',#1570,.T.);
#1074=FACE_OUTER_BOUND('',#1571,.T.);
#1075=FACE_OUTER_BOUND('',#1572,.T.);
#1076=FACE_OUTER_BOUND('',#1573,.T.);
#1077=FACE_OUTER_BOUND('',#1575,.T.);
#1078=FACE_OUTER_BOUND('',#1577,.T.);
#1079=FACE_OUTER_BOUND('',#1578,.T.);
#1080=FACE_OUTER_BOUND('',#1579,.T.);
#1081=FACE_OUTER_BOUND('',#1580,.T.);
#1082=FACE_OUTER_BOUND('',#1581,.T.);
#1083=FACE_OUTER_BOUND('',#1582,.T.);
#1084=FACE_OUTER_BOUND('',#1583,.T.);
#1085=FACE_OUTER_BOUND('',#1584,.T.);
#1086=FACE_OUTER_BOUND('',#1585,.T.);
#1087=FACE_OUTER_BOUND('',#1586,.T.);
#1088=FACE_OUTER_BOUND('',#1587,.T.);
#1089=FACE_OUTER_BOUND('',#1589,.T.);
#1090=FACE_OUTER_BOUND('',#1590,.T.);
#1091=FACE_OUTER_BOUND('',#1591,.T.);
#1092=FACE_OUTER_BOUND('',#1592,.T.);
#1093=FACE_OUTER_BOUND('',#1593,.T.);
#1094=FACE_OUTER_BOUND('',#1594,.T.);
#1095=FACE_OUTER_BOUND('',#1595,.T.);
#1096=FACE_OUTER_BOUND('',#1596,.T.);
#1097=FACE_OUTER_BOUND('',#1597,.T.);
#1098=FACE_OUTER_BOUND('',#1598,.T.);
#1099=FACE_OUTER_BOUND('',#1599,.T.);
#1100=FACE_OUTER_BOUND('',#1600,.T.);
#1101=FACE_OUTER_BOUND('',#1601,.T.);
#1102=FACE_OUTER_BOUND('',#1602,.T.);
#1103=FACE_OUTER_BOUND('',#1603,.T.);
#1104=FACE_OUTER_BOUND('',#1604,.T.);
#1105=FACE_OUTER_BOUND('',#1605,.T.);
#1106=FACE_OUTER_BOUND('',#1606,.T.);
#1107=FACE_OUTER_BOUND('',#1607,.T.);
#1108=FACE_OUTER_BOUND('',#1608,.T.);
#1109=FACE_OUTER_BOUND('',#1612,.T.);
#1110=FACE_OUTER_BOUND('',#1613,.T.);
#1111=FACE_OUTER_BOUND('',#1614,.T.);
#1112=FACE_OUTER_BOUND('',#1615,.T.);
#1113=FACE_OUTER_BOUND('',#1616,.T.);
#1114=FACE_OUTER_BOUND('',#1617,.T.);
#1115=FACE_OUTER_BOUND('',#1618,.T.);
#1116=FACE_OUTER_BOUND('',#1619,.T.);
#1117=FACE_OUTER_BOUND('',#1620,.T.);
#1118=FACE_OUTER_BOUND('',#1621,.T.);
#1119=FACE_OUTER_BOUND('',#1622,.T.);
#1120=FACE_OUTER_BOUND('',#1623,.T.);
#1121=FACE_OUTER_BOUND('',#1624,.T.);
#1122=FACE_OUTER_BOUND('',#1625,.T.);
#1123=FACE_OUTER_BOUND('',#1626,.T.);
#1124=FACE_OUTER_BOUND('',#1627,.T.);
#1125=FACE_OUTER_BOUND('',#1628,.T.);
#1126=FACE_OUTER_BOUND('',#1629,.T.);
#1127=FACE_OUTER_BOUND('',#1630,.T.);
#1128=FACE_OUTER_BOUND('',#1631,.T.);
#1129=FACE_OUTER_BOUND('',#1632,.T.);
#1130=FACE_OUTER_BOUND('',#1633,.T.);
#1131=FACE_OUTER_BOUND('',#1634,.T.);
#1132=FACE_OUTER_BOUND('',#1635,.T.);
#1133=FACE_OUTER_BOUND('',#1636,.T.);
#1134=FACE_OUTER_BOUND('',#1637,.T.);
#1135=FACE_OUTER_BOUND('',#1638,.T.);
#1136=FACE_OUTER_BOUND('',#1639,.T.);
#1137=FACE_OUTER_BOUND('',#1640,.T.);
#1138=FACE_OUTER_BOUND('',#1641,.T.);
#1139=FACE_OUTER_BOUND('',#1642,.T.);
#1140=FACE_OUTER_BOUND('',#1643,.T.);
#1141=FACE_OUTER_BOUND('',#1644,.T.);
#1142=FACE_OUTER_BOUND('',#1645,.T.);
#1143=FACE_OUTER_BOUND('',#1652,.T.);
#1144=FACE_OUTER_BOUND('',#1653,.T.);
#1145=FACE_OUTER_BOUND('',#1654,.T.);
#1146=FACE_OUTER_BOUND('',#1655,.T.);
#1147=FACE_OUTER_BOUND('',#1656,.T.);
#1148=FACE_OUTER_BOUND('',#1657,.T.);
#1149=FACE_OUTER_BOUND('',#1658,.T.);
#1150=FACE_OUTER_BOUND('',#1659,.T.);
#1151=FACE_OUTER_BOUND('',#1660,.T.);
#1152=FACE_OUTER_BOUND('',#1664,.T.);
#1153=FACE_OUTER_BOUND('',#1665,.T.);
#1154=FACE_OUTER_BOUND('',#1666,.T.);
#1155=FACE_OUTER_BOUND('',#1667,.T.);
#1156=FACE_OUTER_BOUND('',#1668,.T.);
#1157=FACE_OUTER_BOUND('',#1669,.T.);
#1158=FACE_OUTER_BOUND('',#1670,.T.);
#1159=FACE_OUTER_BOUND('',#1672,.T.);
#1160=FACE_OUTER_BOUND('',#1673,.T.);
#1161=FACE_OUTER_BOUND('',#1674,.T.);
#1162=FACE_OUTER_BOUND('',#1675,.T.);
#1163=FACE_OUTER_BOUND('',#1676,.T.);
#1164=FACE_OUTER_BOUND('',#1677,.T.);
#1165=FACE_OUTER_BOUND('',#1678,.T.);
#1166=FACE_OUTER_BOUND('',#1680,.T.);
#1167=FACE_OUTER_BOUND('',#1681,.T.);
#1168=FACE_OUTER_BOUND('',#1682,.T.);
#1169=FACE_OUTER_BOUND('',#1683,.T.);
#1170=FACE_OUTER_BOUND('',#1684,.T.);
#1171=FACE_OUTER_BOUND('',#1685,.T.);
#1172=FACE_OUTER_BOUND('',#1686,.T.);
#1173=FACE_OUTER_BOUND('',#1687,.T.);
#1174=FACE_OUTER_BOUND('',#1688,.T.);
#1175=FACE_OUTER_BOUND('',#1689,.T.);
#1176=FACE_OUTER_BOUND('',#1690,.T.);
#1177=FACE_OUTER_BOUND('',#1691,.T.);
#1178=FACE_OUTER_BOUND('',#1692,.T.);
#1179=FACE_OUTER_BOUND('',#1693,.T.);
#1180=FACE_OUTER_BOUND('',#1695,.T.);
#1181=FACE_OUTER_BOUND('',#1697,.T.);
#1182=FACE_OUTER_BOUND('',#1698,.T.);
#1183=FACE_OUTER_BOUND('',#1699,.T.);
#1184=FACE_OUTER_BOUND('',#1700,.T.);
#1185=FACE_OUTER_BOUND('',#1701,.T.);
#1186=FACE_OUTER_BOUND('',#1702,.T.);
#1187=FACE_OUTER_BOUND('',#1703,.T.);
#1188=FACE_OUTER_BOUND('',#1704,.T.);
#1189=FACE_OUTER_BOUND('',#1705,.T.);
#1190=FACE_OUTER_BOUND('',#1706,.T.);
#1191=FACE_OUTER_BOUND('',#1707,.T.);
#1192=FACE_OUTER_BOUND('',#1709,.T.);
#1193=FACE_OUTER_BOUND('',#1710,.T.);
#1194=FACE_OUTER_BOUND('',#1711,.T.);
#1195=FACE_OUTER_BOUND('',#1712,.T.);
#1196=FACE_OUTER_BOUND('',#1713,.T.);
#1197=FACE_OUTER_BOUND('',#1714,.T.);
#1198=FACE_OUTER_BOUND('',#1715,.T.);
#1199=FACE_OUTER_BOUND('',#1716,.T.);
#1200=FACE_OUTER_BOUND('',#1717,.T.);
#1201=FACE_OUTER_BOUND('',#1718,.T.);
#1202=FACE_OUTER_BOUND('',#1719,.T.);
#1203=FACE_OUTER_BOUND('',#1720,.T.);
#1204=FACE_OUTER_BOUND('',#1721,.T.);
#1205=FACE_OUTER_BOUND('',#1722,.T.);
#1206=FACE_OUTER_BOUND('',#1723,.T.);
#1207=FACE_OUTER_BOUND('',#1724,.T.);
#1208=FACE_OUTER_BOUND('',#1725,.T.);
#1209=FACE_OUTER_BOUND('',#1726,.T.);
#1210=FACE_OUTER_BOUND('',#1727,.T.);
#1211=FACE_OUTER_BOUND('',#1728,.T.);
#1212=FACE_OUTER_BOUND('',#1732,.T.);
#1213=FACE_OUTER_BOUND('',#1733,.T.);
#1214=FACE_OUTER_BOUND('',#1734,.T.);
#1215=FACE_OUTER_BOUND('',#1735,.T.);
#1216=FACE_OUTER_BOUND('',#1736,.T.);
#1217=FACE_OUTER_BOUND('',#1737,.T.);
#1218=FACE_OUTER_BOUND('',#1738,.T.);
#1219=FACE_OUTER_BOUND('',#1739,.T.);
#1220=FACE_OUTER_BOUND('',#1740,.T.);
#1221=FACE_OUTER_BOUND('',#1741,.T.);
#1222=FACE_OUTER_BOUND('',#1742,.T.);
#1223=FACE_OUTER_BOUND('',#1743,.T.);
#1224=FACE_OUTER_BOUND('',#1744,.T.);
#1225=FACE_OUTER_BOUND('',#1745,.T.);
#1226=FACE_OUTER_BOUND('',#1746,.T.);
#1227=FACE_OUTER_BOUND('',#1747,.T.);
#1228=FACE_OUTER_BOUND('',#1748,.T.);
#1229=FACE_OUTER_BOUND('',#1749,.T.);
#1230=FACE_OUTER_BOUND('',#1750,.T.);
#1231=FACE_OUTER_BOUND('',#1751,.T.);
#1232=FACE_OUTER_BOUND('',#1752,.T.);
#1233=FACE_OUTER_BOUND('',#1753,.T.);
#1234=FACE_OUTER_BOUND('',#1754,.T.);
#1235=FACE_OUTER_BOUND('',#1755,.T.);
#1236=FACE_OUTER_BOUND('',#1756,.T.);
#1237=FACE_OUTER_BOUND('',#1757,.T.);
#1238=FACE_OUTER_BOUND('',#1758,.T.);
#1239=FACE_OUTER_BOUND('',#1759,.T.);
#1240=FACE_OUTER_BOUND('',#1760,.T.);
#1241=FACE_OUTER_BOUND('',#1761,.T.);
#1242=FACE_OUTER_BOUND('',#1762,.T.);
#1243=FACE_OUTER_BOUND('',#1763,.T.);
#1244=FACE_OUTER_BOUND('',#1764,.T.);
#1245=FACE_OUTER_BOUND('',#1765,.T.);
#1246=FACE_OUTER_BOUND('',#1772,.T.);
#1247=FACE_OUTER_BOUND('',#1773,.T.);
#1248=FACE_OUTER_BOUND('',#1774,.T.);
#1249=FACE_OUTER_BOUND('',#1775,.T.);
#1250=FACE_OUTER_BOUND('',#1776,.T.);
#1251=FACE_OUTER_BOUND('',#1777,.T.);
#1252=FACE_OUTER_BOUND('',#1778,.T.);
#1253=FACE_OUTER_BOUND('',#1779,.T.);
#1254=FACE_OUTER_BOUND('',#1780,.T.);
#1255=FACE_OUTER_BOUND('',#1781,.T.);
#1256=FACE_OUTER_BOUND('',#1782,.T.);
#1257=FACE_OUTER_BOUND('',#1783,.T.);
#1258=FACE_OUTER_BOUND('',#1784,.T.);
#1259=FACE_OUTER_BOUND('',#1785,.T.);
#1260=FACE_OUTER_BOUND('',#1786,.T.);
#1261=FACE_OUTER_BOUND('',#1787,.T.);
#1262=FACE_OUTER_BOUND('',#1788,.T.);
#1263=FACE_OUTER_BOUND('',#1789,.T.);
#1264=FACE_OUTER_BOUND('',#1790,.T.);
#1265=FACE_OUTER_BOUND('',#1791,.T.);
#1266=FACE_OUTER_BOUND('',#1792,.T.);
#1267=FACE_OUTER_BOUND('',#1793,.T.);
#1268=FACE_OUTER_BOUND('',#1794,.T.);
#1269=FACE_OUTER_BOUND('',#1795,.T.);
#1270=FACE_OUTER_BOUND('',#1796,.T.);
#1271=FACE_OUTER_BOUND('',#1797,.T.);
#1272=FACE_OUTER_BOUND('',#1798,.T.);
#1273=FACE_OUTER_BOUND('',#1799,.T.);
#1274=FACE_OUTER_BOUND('',#1800,.T.);
#1275=FACE_OUTER_BOUND('',#1801,.T.);
#1276=FACE_OUTER_BOUND('',#1802,.T.);
#1277=FACE_OUTER_BOUND('',#1803,.T.);
#1278=FACE_OUTER_BOUND('',#1804,.T.);
#1279=FACE_OUTER_BOUND('',#1805,.T.);
#1280=FACE_OUTER_BOUND('',#1806,.T.);
#1281=FACE_OUTER_BOUND('',#1807,.T.);
#1282=FACE_OUTER_BOUND('',#1808,.T.);
#1283=FACE_OUTER_BOUND('',#1809,.T.);
#1284=FACE_OUTER_BOUND('',#1810,.T.);
#1285=FACE_OUTER_BOUND('',#1811,.T.);
#1286=FACE_OUTER_BOUND('',#1812,.T.);
#1287=FACE_OUTER_BOUND('',#1813,.T.);
#1288=FACE_OUTER_BOUND('',#1814,.T.);
#1289=FACE_OUTER_BOUND('',#1815,.T.);
#1290=FACE_OUTER_BOUND('',#1816,.T.);
#1291=FACE_OUTER_BOUND('',#1817,.T.);
#1292=FACE_OUTER_BOUND('',#1818,.T.);
#1293=FACE_OUTER_BOUND('',#1819,.T.);
#1294=FACE_OUTER_BOUND('',#1820,.T.);
#1295=FACE_OUTER_BOUND('',#1821,.T.);
#1296=FACE_OUTER_BOUND('',#1822,.T.);
#1297=FACE_OUTER_BOUND('',#1823,.T.);
#1298=FACE_OUTER_BOUND('',#1824,.T.);
#1299=FACE_OUTER_BOUND('',#1825,.T.);
#1300=FACE_OUTER_BOUND('',#1826,.T.);
#1301=FACE_OUTER_BOUND('',#1827,.T.);
#1302=FACE_OUTER_BOUND('',#1828,.T.);
#1303=FACE_OUTER_BOUND('',#1829,.T.);
#1304=FACE_OUTER_BOUND('',#1830,.T.);
#1305=FACE_OUTER_BOUND('',#1831,.T.);
#1306=FACE_OUTER_BOUND('',#1832,.T.);
#1307=FACE_OUTER_BOUND('',#1833,.T.);
#1308=FACE_OUTER_BOUND('',#1834,.T.);
#1309=FACE_OUTER_BOUND('',#1835,.T.);
#1310=FACE_OUTER_BOUND('',#1836,.T.);
#1311=FACE_OUTER_BOUND('',#1837,.T.);
#1312=FACE_OUTER_BOUND('',#1838,.T.);
#1313=FACE_OUTER_BOUND('',#1839,.T.);
#1314=FACE_OUTER_BOUND('',#1840,.T.);
#1315=FACE_OUTER_BOUND('',#1841,.T.);
#1316=FACE_OUTER_BOUND('',#1842,.T.);
#1317=FACE_OUTER_BOUND('',#1843,.T.);
#1318=FACE_OUTER_BOUND('',#1844,.T.);
#1319=FACE_OUTER_BOUND('',#1845,.T.);
#1320=FACE_OUTER_BOUND('',#1846,.T.);
#1321=FACE_OUTER_BOUND('',#1848,.T.);
#1322=FACE_OUTER_BOUND('',#1849,.T.);
#1323=FACE_OUTER_BOUND('',#1851,.T.);
#1324=FACE_OUTER_BOUND('',#1852,.T.);
#1325=FACE_OUTER_BOUND('',#1853,.T.);
#1326=FACE_OUTER_BOUND('',#1854,.T.);
#1327=FACE_OUTER_BOUND('',#1855,.T.);
#1328=FACE_OUTER_BOUND('',#1856,.T.);
#1329=FACE_OUTER_BOUND('',#1857,.T.);
#1330=FACE_OUTER_BOUND('',#1858,.T.);
#1331=FACE_OUTER_BOUND('',#1859,.T.);
#1332=FACE_OUTER_BOUND('',#1860,.T.);
#1333=FACE_OUTER_BOUND('',#1861,.T.);
#1334=FACE_OUTER_BOUND('',#1862,.T.);
#1335=FACE_OUTER_BOUND('',#1863,.T.);
#1336=FACE_OUTER_BOUND('',#1864,.T.);
#1337=FACE_OUTER_BOUND('',#1865,.T.);
#1338=FACE_OUTER_BOUND('',#1867,.T.);
#1339=FACE_OUTER_BOUND('',#1868,.T.);
#1340=FACE_OUTER_BOUND('',#1869,.T.);
#1341=FACE_OUTER_BOUND('',#1870,.T.);
#1342=FACE_OUTER_BOUND('',#1871,.T.);
#1343=FACE_OUTER_BOUND('',#1872,.T.);
#1344=FACE_OUTER_BOUND('',#1873,.T.);
#1345=FACE_OUTER_BOUND('',#1874,.T.);
#1346=FACE_OUTER_BOUND('',#1876,.T.);
#1347=FACE_OUTER_BOUND('',#1877,.T.);
#1348=FACE_OUTER_BOUND('',#1878,.T.);
#1349=FACE_OUTER_BOUND('',#1880,.T.);
#1350=FACE_OUTER_BOUND('',#1881,.T.);
#1351=FACE_OUTER_BOUND('',#1882,.T.);
#1352=FACE_OUTER_BOUND('',#1884,.T.);
#1353=FACE_OUTER_BOUND('',#1885,.T.);
#1354=FACE_OUTER_BOUND('',#1886,.T.);
#1355=FACE_OUTER_BOUND('',#1888,.T.);
#1356=FACE_OUTER_BOUND('',#1889,.T.);
#1357=FACE_OUTER_BOUND('',#1890,.T.);
#1358=FACE_OUTER_BOUND('',#1892,.T.);
#1359=FACE_OUTER_BOUND('',#1893,.T.);
#1360=FACE_OUTER_BOUND('',#1894,.T.);
#1361=FACE_OUTER_BOUND('',#1895,.T.);
#1362=FACE_OUTER_BOUND('',#1896,.T.);
#1363=FACE_OUTER_BOUND('',#1897,.T.);
#1364=FACE_OUTER_BOUND('',#1898,.T.);
#1365=FACE_OUTER_BOUND('',#1899,.T.);
#1366=FACE_OUTER_BOUND('',#1900,.T.);
#1367=FACE_OUTER_BOUND('',#1901,.T.);
#1368=FACE_OUTER_BOUND('',#1902,.T.);
#1369=FACE_OUTER_BOUND('',#1903,.T.);
#1370=FACE_OUTER_BOUND('',#1904,.T.);
#1371=FACE_OUTER_BOUND('',#1905,.T.);
#1372=FACE_OUTER_BOUND('',#1906,.T.);
#1373=FACE_OUTER_BOUND('',#1907,.T.);
#1374=FACE_OUTER_BOUND('',#1908,.T.);
#1375=FACE_OUTER_BOUND('',#1909,.T.);
#1376=FACE_OUTER_BOUND('',#1910,.T.);
#1377=FACE_OUTER_BOUND('',#1913,.T.);
#1378=FACE_OUTER_BOUND('',#1914,.T.);
#1379=FACE_OUTER_BOUND('',#1915,.T.);
#1380=FACE_OUTER_BOUND('',#1916,.T.);
#1381=FACE_OUTER_BOUND('',#1923,.T.);
#1382=FACE_OUTER_BOUND('',#1924,.T.);
#1383=FACE_OUTER_BOUND('',#1925,.T.);
#1384=FACE_OUTER_BOUND('',#1926,.T.);
#1385=FACE_OUTER_BOUND('',#1928,.T.);
#1386=EDGE_LOOP('',(#5646,#5647,#5648,#5649));
#1387=EDGE_LOOP('',(#5650,#5651,#5652,#5653));
#1388=EDGE_LOOP('',(#5654,#5655,#5656,#5657));
#1389=EDGE_LOOP('',(#5658,#5659,#5660,#5661));
#1390=EDGE_LOOP('',(#5662,#5663,#5664,#5665));
#1391=EDGE_LOOP('',(#5666,#5667,#5668,#5669));
#1392=EDGE_LOOP('',(#5670,#5671,#5672,#5673));
#1393=EDGE_LOOP('',(#5674,#5675,#5676,#5677));
#1394=EDGE_LOOP('',(#5678,#5679,#5680,#5681));
#1395=EDGE_LOOP('',(#5682,#5683,#5684,#5685));
#1396=EDGE_LOOP('',(#5686,#5687,#5688,#5689));
#1397=EDGE_LOOP('',(#5690,#5691,#5692,#5693));
#1398=EDGE_LOOP('',(#5694,#5695,#5696,#5697));
#1399=EDGE_LOOP('',(#5698,#5699,#5700,#5701));
#1400=EDGE_LOOP('',(#5702,#5703,#5704,#5705));
#1401=EDGE_LOOP('',(#5706,#5707,#5708,#5709));
#1402=EDGE_LOOP('',(#5710,#5711,#5712,#5713));
#1403=EDGE_LOOP('',(#5714,#5715,#5716,#5717));
#1404=EDGE_LOOP('',(#5718,#5719,#5720,#5721));
#1405=EDGE_LOOP('',(#5722,#5723,#5724,#5725));
#1406=EDGE_LOOP('',(#5726,#5727,#5728,#5729));
#1407=EDGE_LOOP('',(#5730,#5731,#5732,#5733));
#1408=EDGE_LOOP('',(#5734,#5735,#5736,#5737));
#1409=EDGE_LOOP('',(#5738,#5739,#5740,#5741));
#1410=EDGE_LOOP('',(#5742,#5743,#5744,#5745));
#1411=EDGE_LOOP('',(#5746,#5747,#5748,#5749));
#1412=EDGE_LOOP('',(#5750,#5751,#5752,#5753));
#1413=EDGE_LOOP('',(#5754,#5755,#5756,#5757));
#1414=EDGE_LOOP('',(#5758,#5759,#5760,#5761));
#1415=EDGE_LOOP('',(#5762,#5763,#5764,#5765));
#1416=EDGE_LOOP('',(#5766,#5767,#5768,#5769));
#1417=EDGE_LOOP('',(#5770,#5771,#5772,#5773));
#1418=EDGE_LOOP('',(#5774,#5775,#5776,#5777));
#1419=EDGE_LOOP('',(#5778,#5779,#5780,#5781));
#1420=EDGE_LOOP('',(#5782,#5783,#5784,#5785));
#1421=EDGE_LOOP('',(#5786,#5787,#5788,#5789));
#1422=EDGE_LOOP('',(#5790,#5791,#5792,#5793));
#1423=EDGE_LOOP('',(#5794,#5795,#5796,#5797));
#1424=EDGE_LOOP('',(#5798,#5799,#5800,#5801));
#1425=EDGE_LOOP('',(#5802,#5803,#5804,#5805));
#1426=EDGE_LOOP('',(#5806,#5807,#5808,#5809));
#1427=EDGE_LOOP('',(#5810,#5811,#5812,#5813));
#1428=EDGE_LOOP('',(#5814,#5815,#5816,#5817));
#1429=EDGE_LOOP('',(#5818,#5819,#5820,#5821));
#1430=EDGE_LOOP('',(#5822,#5823,#5824,#5825));
#1431=EDGE_LOOP('',(#5826,#5827,#5828,#5829));
#1432=EDGE_LOOP('',(#5830,#5831,#5832,#5833));
#1433=EDGE_LOOP('',(#5834,#5835,#5836,#5837));
#1434=EDGE_LOOP('',(#5838,#5839,#5840,#5841));
#1435=EDGE_LOOP('',(#5842,#5843,#5844,#5845));
#1436=EDGE_LOOP('',(#5846,#5847,#5848,#5849));
#1437=EDGE_LOOP('',(#5850,#5851,#5852,#5853));
#1438=EDGE_LOOP('',(#5854,#5855,#5856,#5857));
#1439=EDGE_LOOP('',(#5858,#5859,#5860,#5861));
#1440=EDGE_LOOP('',(#5862,#5863,#5864,#5865));
#1441=EDGE_LOOP('',(#5866,#5867,#5868,#5869));
#1442=EDGE_LOOP('',(#5870,#5871,#5872,#5873));
#1443=EDGE_LOOP('',(#5874,#5875,#5876,#5877));
#1444=EDGE_LOOP('',(#5878,#5879,#5880,#5881));
#1445=EDGE_LOOP('',(#5882,#5883,#5884,#5885));
#1446=EDGE_LOOP('',(#5886,#5887,#5888,#5889));
#1447=EDGE_LOOP('',(#5890,#5891,#5892,#5893));
#1448=EDGE_LOOP('',(#5894,#5895,#5896,#5897));
#1449=EDGE_LOOP('',(#5898,#5899,#5900,#5901));
#1450=EDGE_LOOP('',(#5902,#5903,#5904,#5905));
#1451=EDGE_LOOP('',(#5906,#5907,#5908,#5909));
#1452=EDGE_LOOP('',(#5910,#5911,#5912,#5913));
#1453=EDGE_LOOP('',(#5914,#5915,#5916,#5917));
#1454=EDGE_LOOP('',(#5918,#5919,#5920,#5921));
#1455=EDGE_LOOP('',(#5922,#5923,#5924,#5925));
#1456=EDGE_LOOP('',(#5926,#5927,#5928,#5929));
#1457=EDGE_LOOP('',(#5930,#5931,#5932,#5933));
#1458=EDGE_LOOP('',(#5934,#5935,#5936,#5937));
#1459=EDGE_LOOP('',(#5938,#5939,#5940,#5941));
#1460=EDGE_LOOP('',(#5942,#5943,#5944,#5945));
#1461=EDGE_LOOP('',(#5946,#5947,#5948,#5949));
#1462=EDGE_LOOP('',(#5950,#5951,#5952,#5953));
#1463=EDGE_LOOP('',(#5954,#5955,#5956,#5957));
#1464=EDGE_LOOP('',(#5958,#5959,#5960,#5961));
#1465=EDGE_LOOP('',(#5962,#5963,#5964,#5965,#5966,#5967));
#1466=EDGE_LOOP('',(#5968,#5969,#5970,#5971));
#1467=EDGE_LOOP('',(#5972,#5973,#5974,#5975));
#1468=EDGE_LOOP('',(#5976,#5977,#5978,#5979));
#1469=EDGE_LOOP('',(#5980,#5981,#5982,#5983));
#1470=EDGE_LOOP('',(#5984,#5985,#5986,#5987));
#1471=EDGE_LOOP('',(#5988,#5989,#5990,#5991));
#1472=EDGE_LOOP('',(#5992,#5993,#5994,#5995));
#1473=EDGE_LOOP('',(#5996,#5997,#5998,#5999));
#1474=EDGE_LOOP('',(#6000,#6001,#6002,#6003));
#1475=EDGE_LOOP('',(#6004,#6005,#6006,#6007));
#1476=EDGE_LOOP('',(#6008,#6009,#6010,#6011));
#1477=EDGE_LOOP('',(#6012,#6013,#6014,#6015));
#1478=EDGE_LOOP('',(#6016,#6017,#6018,#6019));
#1479=EDGE_LOOP('',(#6020,#6021,#6022,#6023));
#1480=EDGE_LOOP('',(#6024,#6025,#6026,#6027));
#1481=EDGE_LOOP('',(#6028,#6029,#6030,#6031));
#1482=EDGE_LOOP('',(#6032,#6033,#6034,#6035));
#1483=EDGE_LOOP('',(#6036,#6037,#6038,#6039));
#1484=EDGE_LOOP('',(#6040,#6041,#6042,#6043));
#1485=EDGE_LOOP('',(#6044,#6045,#6046,#6047));
#1486=EDGE_LOOP('',(#6048,#6049,#6050,#6051));
#1487=EDGE_LOOP('',(#6052,#6053,#6054,#6055));
#1488=EDGE_LOOP('',(#6056,#6057,#6058,#6059));
#1489=EDGE_LOOP('',(#6060,#6061,#6062,#6063));
#1490=EDGE_LOOP('',(#6064,#6065,#6066,#6067));
#1491=EDGE_LOOP('',(#6068,#6069,#6070,#6071));
#1492=EDGE_LOOP('',(#6072,#6073,#6074,#6075));
#1493=EDGE_LOOP('',(#6076,#6077,#6078,#6079));
#1494=EDGE_LOOP('',(#6080,#6081,#6082,#6083));
#1495=EDGE_LOOP('',(#6084,#6085,#6086,#6087));
#1496=EDGE_LOOP('',(#6088,#6089,#6090,#6091));
#1497=EDGE_LOOP('',(#6092,#6093,#6094,#6095));
#1498=EDGE_LOOP('',(#6096,#6097,#6098,#6099));
#1499=EDGE_LOOP('',(#6100,#6101,#6102,#6103));
#1500=EDGE_LOOP('',(#6104,#6105,#6106,#6107));
#1501=EDGE_LOOP('',(#6108,#6109,#6110,#6111));
#1502=EDGE_LOOP('',(#6112,#6113,#6114,#6115));
#1503=EDGE_LOOP('',(#6116,#6117,#6118,#6119));
#1504=EDGE_LOOP('',(#6120,#6121,#6122,#6123,#6124,#6125,#6126,#6127,#6128,
#6129,#6130,#6131,#6132,#6133,#6134,#6135,#6136,#6137,#6138,#6139,#6140,
#6141,#6142,#6143,#6144,#6145,#6146,#6147,#6148,#6149,#6150,#6151,#6152,
#6153,#6154,#6155,#6156,#6157,#6158,#6159,#6160,#6161,#6162,#6163,#6164,
#6165,#6166,#6167,#6168,#6169,#6170,#6171,#6172,#6173,#6174,#6175,#6176,
#6177,#6178,#6179,#6180,#6181,#6182,#6183,#6184,#6185,#6186,#6187,#6188,
#6189,#6190,#6191,#6192,#6193,#6194,#6195,#6196,#6197,#6198,#6199,#6200,
#6201,#6202,#6203,#6204,#6205,#6206,#6207,#6208,#6209,#6210,#6211,#6212,
#6213,#6214,#6215,#6216,#6217,#6218,#6219,#6220,#6221,#6222,#6223,#6224,
#6225,#6226,#6227,#6228,#6229,#6230,#6231,#6232,#6233,#6234,#6235,#6236,
#6237,#6238));
#1505=EDGE_LOOP('',(#6239,#6240,#6241,#6242));
#1506=EDGE_LOOP('',(#6243,#6244,#6245,#6246));
#1507=EDGE_LOOP('',(#6247,#6248,#6249,#6250));
#1508=EDGE_LOOP('',(#6251,#6252,#6253,#6254));
#1509=EDGE_LOOP('',(#6255,#6256,#6257,#6258,#6259,#6260));
#1510=EDGE_LOOP('',(#6261,#6262,#6263,#6264,#6265,#6266,#6267,#6268,#6269,
#6270,#6271,#6272));
#1511=EDGE_LOOP('',(#6273));
#1512=EDGE_LOOP('',(#6274));
#1513=EDGE_LOOP('',(#6275));
#1514=EDGE_LOOP('',(#6276,#6277,#6278,#6279));
#1515=EDGE_LOOP('',(#6280,#6281,#6282,#6283));
#1516=EDGE_LOOP('',(#6284,#6285,#6286,#6287));
#1517=EDGE_LOOP('',(#6288,#6289,#6290,#6291));
#1518=EDGE_LOOP('',(#6292,#6293,#6294,#6295));
#1519=EDGE_LOOP('',(#6296,#6297,#6298,#6299));
#1520=EDGE_LOOP('',(#6300,#6301,#6302,#6303));
#1521=EDGE_LOOP('',(#6304,#6305,#6306,#6307,#6308,#6309,#6310,#6311,#6312,
#6313,#6314,#6315,#6316,#6317,#6318,#6319,#6320,#6321,#6322,#6323,#6324,
#6325,#6326,#6327,#6328,#6329,#6330,#6331,#6332,#6333,#6334,#6335,#6336,
#6337,#6338,#6339,#6340,#6341,#6342,#6343,#6344,#6345,#6346,#6347,#6348,
#6349,#6350,#6351,#6352,#6353,#6354,#6355,#6356,#6357,#6358,#6359,#6360,
#6361,#6362,#6363,#6364,#6365,#6366,#6367,#6368,#6369,#6370,#6371,#6372,
#6373,#6374,#6375,#6376,#6377,#6378,#6379,#6380,#6381,#6382,#6383,#6384,
#6385,#6386,#6387,#6388,#6389,#6390,#6391,#6392,#6393,#6394,#6395,#6396,
#6397,#6398,#6399,#6400,#6401,#6402,#6403,#6404,#6405,#6406,#6407,#6408,
#6409,#6410,#6411,#6412,#6413,#6414,#6415,#6416,#6417,#6418,#6419,#6420,
#6421,#6422,#6423,#6424,#6425,#6426,#6427,#6428,#6429,#6430));
#1522=EDGE_LOOP('',(#6431));
#1523=EDGE_LOOP('',(#6432));
#1524=EDGE_LOOP('',(#6433));
#1525=EDGE_LOOP('',(#6434,#6435,#6436,#6437));
#1526=EDGE_LOOP('',(#6438,#6439,#6440,#6441));
#1527=EDGE_LOOP('',(#6442));
#1528=EDGE_LOOP('',(#6443));
#1529=EDGE_LOOP('',(#6444));
#1530=EDGE_LOOP('',(#6445));
#1531=EDGE_LOOP('',(#6446,#6447,#6448,#6449));
#1532=EDGE_LOOP('',(#6450));
#1533=EDGE_LOOP('',(#6451));
#1534=EDGE_LOOP('',(#6452,#6453,#6454,#6455));
#1535=EDGE_LOOP('',(#6456));
#1536=EDGE_LOOP('',(#6457,#6458,#6459,#6460));
#1537=EDGE_LOOP('',(#6461));
#1538=EDGE_LOOP('',(#6462,#6463,#6464,#6465));
#1539=EDGE_LOOP('',(#6466,#6467,#6468,#6469));
#1540=EDGE_LOOP('',(#6470,#6471,#6472,#6473));
#1541=EDGE_LOOP('',(#6474,#6475,#6476,#6477));
#1542=EDGE_LOOP('',(#6478,#6479,#6480,#6481));
#1543=EDGE_LOOP('',(#6482,#6483,#6484,#6485));
#1544=EDGE_LOOP('',(#6486,#6487));
#1545=EDGE_LOOP('',(#6488,#6489));
#1546=EDGE_LOOP('',(#6490,#6491));
#1547=EDGE_LOOP('',(#6492,#6493));
#1548=EDGE_LOOP('',(#6494,#6495,#6496,#6497,#6498,#6499));
#1549=EDGE_LOOP('',(#6500,#6501,#6502,#6503,#6504,#6505));
#1550=EDGE_LOOP('',(#6506,#6507,#6508,#6509,#6510,#6511,#6512,#6513));
#1551=EDGE_LOOP('',(#6514));
#1552=EDGE_LOOP('',(#6515));
#1553=EDGE_LOOP('',(#6516));
#1554=EDGE_LOOP('',(#6517,#6518,#6519,#6520));
#1555=EDGE_LOOP('',(#6521,#6522,#6523,#6524));
#1556=EDGE_LOOP('',(#6525,#6526,#6527,#6528));
#1557=EDGE_LOOP('',(#6529,#6530,#6531,#6532));
#1558=EDGE_LOOP('',(#6533,#6534,#6535,#6536));
#1559=EDGE_LOOP('',(#6537));
#1560=EDGE_LOOP('',(#6538));
#1561=EDGE_LOOP('',(#6539,#6540,#6541,#6542));
#1562=EDGE_LOOP('',(#6543));
#1563=EDGE_LOOP('',(#6544));
#1564=EDGE_LOOP('',(#6545,#6546,#6547,#6548));
#1565=EDGE_LOOP('',(#6549,#6550,#6551,#6552));
#1566=EDGE_LOOP('',(#6553,#6554,#6555,#6556));
#1567=EDGE_LOOP('',(#6557,#6558,#6559,#6560));
#1568=EDGE_LOOP('',(#6561,#6562,#6563,#6564));
#1569=EDGE_LOOP('',(#6565,#6566,#6567,#6568));
#1570=EDGE_LOOP('',(#6569,#6570,#6571,#6572));
#1571=EDGE_LOOP('',(#6573,#6574,#6575,#6576));
#1572=EDGE_LOOP('',(#6577,#6578,#6579,#6580));
#1573=EDGE_LOOP('',(#6581));
#1574=EDGE_LOOP('',(#6582));
#1575=EDGE_LOOP('',(#6583));
#1576=EDGE_LOOP('',(#6584));
#1577=EDGE_LOOP('',(#6585,#6586,#6587,#6588));
#1578=EDGE_LOOP('',(#6589,#6590,#6591,#6592));
#1579=EDGE_LOOP('',(#6593,#6594,#6595,#6596));
#1580=EDGE_LOOP('',(#6597,#6598,#6599,#6600));
#1581=EDGE_LOOP('',(#6601,#6602,#6603,#6604));
#1582=EDGE_LOOP('',(#6605,#6606,#6607,#6608,#6609,#6610));
#1583=EDGE_LOOP('',(#6611,#6612,#6613,#6614,#6615,#6616,#6617,#6618,#6619,
#6620));
#1584=EDGE_LOOP('',(#6621,#6622,#6623,#6624,#6625,#6626,#6627,#6628,#6629,
#6630));
#1585=EDGE_LOOP('',(#6631,#6632,#6633,#6634,#6635,#6636,#6637,#6638,#6639,
#6640));
#1586=EDGE_LOOP('',(#6641,#6642,#6643,#6644,#6645,#6646,#6647,#6648));
#1587=EDGE_LOOP('',(#6649,#6650,#6651,#6652,#6653,#6654,#6655,#6656,#6657,
#6658,#6659,#6660,#6661,#6662,#6663,#6664,#6665,#6666,#6667,#6668,#6669,
#6670,#6671,#6672,#6673,#6674,#6675,#6676,#6677,#6678,#6679,#6680,#6681,
#6682,#6683,#6684,#6685,#6686,#6687,#6688,#6689,#6690));
#1588=EDGE_LOOP('',(#6691,#6692,#6693,#6694,#6695,#6696));
#1589=EDGE_LOOP('',(#6697,#6698,#6699,#6700));
#1590=EDGE_LOOP('',(#6701,#6702,#6703,#6704));
#1591=EDGE_LOOP('',(#6705,#6706,#6707,#6708,#6709,#6710));
#1592=EDGE_LOOP('',(#6711,#6712,#6713,#6714));
#1593=EDGE_LOOP('',(#6715,#6716,#6717,#6718));
#1594=EDGE_LOOP('',(#6719,#6720,#6721,#6722,#6723,#6724));
#1595=EDGE_LOOP('',(#6725,#6726,#6727,#6728));
#1596=EDGE_LOOP('',(#6729,#6730,#6731,#6732));
#1597=EDGE_LOOP('',(#6733,#6734,#6735,#6736));
#1598=EDGE_LOOP('',(#6737,#6738,#6739,#6740));
#1599=EDGE_LOOP('',(#6741,#6742,#6743,#6744,#6745,#6746,#6747,#6748,#6749,
#6750));
#1600=EDGE_LOOP('',(#6751,#6752,#6753,#6754));
#1601=EDGE_LOOP('',(#6755,#6756,#6757,#6758));
#1602=EDGE_LOOP('',(#6759,#6760,#6761,#6762));
#1603=EDGE_LOOP('',(#6763,#6764,#6765,#6766));
#1604=EDGE_LOOP('',(#6767,#6768,#6769,#6770));
#1605=EDGE_LOOP('',(#6771,#6772,#6773,#6774,#6775,#6776,#6777,#6778,#6779,
#6780));
#1606=EDGE_LOOP('',(#6781,#6782,#6783,#6784));
#1607=EDGE_LOOP('',(#6785,#6786,#6787,#6788,#6789,#6790));
#1608=EDGE_LOOP('',(#6791,#6792,#6793,#6794,#6795,#6796,#6797,#6798));
#1609=EDGE_LOOP('',(#6799));
#1610=EDGE_LOOP('',(#6800));
#1611=EDGE_LOOP('',(#6801));
#1612=EDGE_LOOP('',(#6802,#6803,#6804,#6805));
#1613=EDGE_LOOP('',(#6806,#6807,#6808,#6809,#6810,#6811,#6812,#6813,#6814,
#6815));
#1614=EDGE_LOOP('',(#6816,#6817,#6818,#6819));
#1615=EDGE_LOOP('',(#6820,#6821,#6822,#6823));
#1616=EDGE_LOOP('',(#6824,#6825,#6826,#6827));
#1617=EDGE_LOOP('',(#6828,#6829,#6830,#6831));
#1618=EDGE_LOOP('',(#6832,#6833,#6834,#6835));
#1619=EDGE_LOOP('',(#6836,#6837,#6838));
#1620=EDGE_LOOP('',(#6839,#6840,#6841));
#1621=EDGE_LOOP('',(#6842,#6843,#6844));
#1622=EDGE_LOOP('',(#6845,#6846,#6847,#6848));
#1623=EDGE_LOOP('',(#6849,#6850,#6851,#6852));
#1624=EDGE_LOOP('',(#6853,#6854,#6855));
#1625=EDGE_LOOP('',(#6856,#6857,#6858,#6859));
#1626=EDGE_LOOP('',(#6860,#6861,#6862,#6863));
#1627=EDGE_LOOP('',(#6864,#6865,#6866,#6867));
#1628=EDGE_LOOP('',(#6868,#6869,#6870,#6871));
#1629=EDGE_LOOP('',(#6872,#6873,#6874,#6875));
#1630=EDGE_LOOP('',(#6876,#6877,#6878,#6879));
#1631=EDGE_LOOP('',(#6880,#6881,#6882));
#1632=EDGE_LOOP('',(#6883,#6884,#6885));
#1633=EDGE_LOOP('',(#6886,#6887,#6888));
#1634=EDGE_LOOP('',(#6889,#6890,#6891,#6892));
#1635=EDGE_LOOP('',(#6893,#6894,#6895,#6896));
#1636=EDGE_LOOP('',(#6897,#6898,#6899));
#1637=EDGE_LOOP('',(#6900,#6901,#6902,#6903));
#1638=EDGE_LOOP('',(#6904,#6905,#6906,#6907));
#1639=EDGE_LOOP('',(#6908,#6909,#6910,#6911));
#1640=EDGE_LOOP('',(#6912,#6913,#6914,#6915));
#1641=EDGE_LOOP('',(#6916,#6917,#6918,#6919));
#1642=EDGE_LOOP('',(#6920,#6921,#6922,#6923));
#1643=EDGE_LOOP('',(#6924,#6925,#6926,#6927));
#1644=EDGE_LOOP('',(#6928,#6929,#6930,#6931,#6932,#6933,#6934,#6935));
#1645=EDGE_LOOP('',(#6936,#6937,#6938,#6939));
#1646=EDGE_LOOP('',(#6940));
#1647=EDGE_LOOP('',(#6941));
#1648=EDGE_LOOP('',(#6942));
#1649=EDGE_LOOP('',(#6943));
#1650=EDGE_LOOP('',(#6944));
#1651=EDGE_LOOP('',(#6945));
#1652=EDGE_LOOP('',(#6946,#6947,#6948,#6949));
#1653=EDGE_LOOP('',(#6950,#6951,#6952,#6953));
#1654=EDGE_LOOP('',(#6954,#6955));
#1655=EDGE_LOOP('',(#6956,#6957));
#1656=EDGE_LOOP('',(#6958,#6959));
#1657=EDGE_LOOP('',(#6960,#6961));
#1658=EDGE_LOOP('',(#6962,#6963,#6964,#6965,#6966,#6967));
#1659=EDGE_LOOP('',(#6968,#6969,#6970,#6971,#6972,#6973));
#1660=EDGE_LOOP('',(#6974,#6975,#6976,#6977,#6978,#6979,#6980,#6981));
#1661=EDGE_LOOP('',(#6982));
#1662=EDGE_LOOP('',(#6983));
#1663=EDGE_LOOP('',(#6984));
#1664=EDGE_LOOP('',(#6985,#6986,#6987,#6988));
#1665=EDGE_LOOP('',(#6989,#6990,#6991,#6992));
#1666=EDGE_LOOP('',(#6993,#6994,#6995,#6996));
#1667=EDGE_LOOP('',(#6997,#6998,#6999,#7000));
#1668=EDGE_LOOP('',(#7001,#7002,#7003,#7004));
#1669=EDGE_LOOP('',(#7005,#7006,#7007,#7008));
#1670=EDGE_LOOP('',(#7009,#7010,#7011,#7012,#7013,#7014));
#1671=EDGE_LOOP('',(#7015));
#1672=EDGE_LOOP('',(#7016,#7017,#7018,#7019));
#1673=EDGE_LOOP('',(#7020,#7021,#7022,#7023));
#1674=EDGE_LOOP('',(#7024,#7025,#7026,#7027));
#1675=EDGE_LOOP('',(#7028,#7029,#7030,#7031));
#1676=EDGE_LOOP('',(#7032,#7033,#7034,#7035));
#1677=EDGE_LOOP('',(#7036,#7037,#7038,#7039));
#1678=EDGE_LOOP('',(#7040,#7041,#7042,#7043,#7044,#7045));
#1679=EDGE_LOOP('',(#7046));
#1680=EDGE_LOOP('',(#7047,#7048,#7049,#7050));
#1681=EDGE_LOOP('',(#7051,#7052,#7053,#7054));
#1682=EDGE_LOOP('',(#7055,#7056,#7057,#7058));
#1683=EDGE_LOOP('',(#7059,#7060,#7061,#7062));
#1684=EDGE_LOOP('',(#7063,#7064,#7065,#7066));
#1685=EDGE_LOOP('',(#7067,#7068,#7069,#7070));
#1686=EDGE_LOOP('',(#7071,#7072,#7073,#7074));
#1687=EDGE_LOOP('',(#7075,#7076,#7077,#7078));
#1688=EDGE_LOOP('',(#7079,#7080,#7081,#7082));
#1689=EDGE_LOOP('',(#7083,#7084,#7085,#7086));
#1690=EDGE_LOOP('',(#7087,#7088,#7089,#7090));
#1691=EDGE_LOOP('',(#7091,#7092,#7093,#7094));
#1692=EDGE_LOOP('',(#7095,#7096,#7097,#7098));
#1693=EDGE_LOOP('',(#7099));
#1694=EDGE_LOOP('',(#7100));
#1695=EDGE_LOOP('',(#7101));
#1696=EDGE_LOOP('',(#7102));
#1697=EDGE_LOOP('',(#7103,#7104,#7105,#7106));
#1698=EDGE_LOOP('',(#7107,#7108,#7109,#7110));
#1699=EDGE_LOOP('',(#7111,#7112,#7113,#7114));
#1700=EDGE_LOOP('',(#7115,#7116,#7117,#7118));
#1701=EDGE_LOOP('',(#7119,#7120,#7121,#7122));
#1702=EDGE_LOOP('',(#7123,#7124,#7125,#7126,#7127,#7128));
#1703=EDGE_LOOP('',(#7129,#7130,#7131,#7132,#7133,#7134,#7135,#7136,#7137,
#7138));
#1704=EDGE_LOOP('',(#7139,#7140,#7141,#7142,#7143,#7144,#7145,#7146,#7147,
#7148));
#1705=EDGE_LOOP('',(#7149,#7150,#7151,#7152,#7153,#7154,#7155,#7156,#7157,
#7158));
#1706=EDGE_LOOP('',(#7159,#7160,#7161,#7162,#7163,#7164,#7165,#7166));
#1707=EDGE_LOOP('',(#7167,#7168,#7169,#7170,#7171,#7172,#7173,#7174,#7175,
#7176,#7177,#7178,#7179,#7180,#7181,#7182,#7183,#7184,#7185,#7186,#7187,
#7188,#7189,#7190,#7191,#7192,#7193,#7194,#7195,#7196,#7197,#7198,#7199,
#7200,#7201,#7202,#7203,#7204,#7205,#7206,#7207,#7208));
#1708=EDGE_LOOP('',(#7209,#7210,#7211,#7212,#7213,#7214));
#1709=EDGE_LOOP('',(#7215,#7216,#7217,#7218));
#1710=EDGE_LOOP('',(#7219,#7220,#7221,#7222));
#1711=EDGE_LOOP('',(#7223,#7224,#7225,#7226,#7227,#7228));
#1712=EDGE_LOOP('',(#7229,#7230,#7231,#7232));
#1713=EDGE_LOOP('',(#7233,#7234,#7235,#7236));
#1714=EDGE_LOOP('',(#7237,#7238,#7239,#7240,#7241,#7242));
#1715=EDGE_LOOP('',(#7243,#7244,#7245,#7246));
#1716=EDGE_LOOP('',(#7247,#7248,#7249,#7250));
#1717=EDGE_LOOP('',(#7251,#7252,#7253,#7254));
#1718=EDGE_LOOP('',(#7255,#7256,#7257,#7258));
#1719=EDGE_LOOP('',(#7259,#7260,#7261,#7262,#7263,#7264,#7265,#7266,#7267,
#7268));
#1720=EDGE_LOOP('',(#7269,#7270,#7271,#7272));
#1721=EDGE_LOOP('',(#7273,#7274,#7275,#7276));
#1722=EDGE_LOOP('',(#7277,#7278,#7279,#7280));
#1723=EDGE_LOOP('',(#7281,#7282,#7283,#7284));
#1724=EDGE_LOOP('',(#7285,#7286,#7287,#7288));
#1725=EDGE_LOOP('',(#7289,#7290,#7291,#7292,#7293,#7294,#7295,#7296,#7297,
#7298));
#1726=EDGE_LOOP('',(#7299,#7300,#7301,#7302));
#1727=EDGE_LOOP('',(#7303,#7304,#7305,#7306,#7307,#7308));
#1728=EDGE_LOOP('',(#7309,#7310,#7311,#7312,#7313,#7314,#7315,#7316));
#1729=EDGE_LOOP('',(#7317));
#1730=EDGE_LOOP('',(#7318));
#1731=EDGE_LOOP('',(#7319));
#1732=EDGE_LOOP('',(#7320,#7321,#7322,#7323));
#1733=EDGE_LOOP('',(#7324,#7325,#7326,#7327,#7328,#7329,#7330,#7331,#7332,
#7333));
#1734=EDGE_LOOP('',(#7334,#7335,#7336,#7337));
#1735=EDGE_LOOP('',(#7338,#7339,#7340,#7341));
#1736=EDGE_LOOP('',(#7342,#7343,#7344,#7345));
#1737=EDGE_LOOP('',(#7346,#7347,#7348,#7349));
#1738=EDGE_LOOP('',(#7350,#7351,#7352,#7353));
#1739=EDGE_LOOP('',(#7354,#7355,#7356));
#1740=EDGE_LOOP('',(#7357,#7358,#7359));
#1741=EDGE_LOOP('',(#7360,#7361,#7362));
#1742=EDGE_LOOP('',(#7363,#7364,#7365,#7366));
#1743=EDGE_LOOP('',(#7367,#7368,#7369,#7370));
#1744=EDGE_LOOP('',(#7371,#7372,#7373));
#1745=EDGE_LOOP('',(#7374,#7375,#7376,#7377));
#1746=EDGE_LOOP('',(#7378,#7379,#7380,#7381));
#1747=EDGE_LOOP('',(#7382,#7383,#7384,#7385));
#1748=EDGE_LOOP('',(#7386,#7387,#7388,#7389));
#1749=EDGE_LOOP('',(#7390,#7391,#7392,#7393));
#1750=EDGE_LOOP('',(#7394,#7395,#7396,#7397));
#1751=EDGE_LOOP('',(#7398,#7399,#7400));
#1752=EDGE_LOOP('',(#7401,#7402,#7403));
#1753=EDGE_LOOP('',(#7404,#7405,#7406));
#1754=EDGE_LOOP('',(#7407,#7408,#7409,#7410));
#1755=EDGE_LOOP('',(#7411,#7412,#7413,#7414));
#1756=EDGE_LOOP('',(#7415,#7416,#7417));
#1757=EDGE_LOOP('',(#7418,#7419,#7420,#7421));
#1758=EDGE_LOOP('',(#7422,#7423,#7424,#7425));
#1759=EDGE_LOOP('',(#7426,#7427,#7428,#7429));
#1760=EDGE_LOOP('',(#7430,#7431,#7432,#7433));
#1761=EDGE_LOOP('',(#7434,#7435,#7436,#7437));
#1762=EDGE_LOOP('',(#7438,#7439,#7440,#7441));
#1763=EDGE_LOOP('',(#7442,#7443,#7444,#7445));
#1764=EDGE_LOOP('',(#7446,#7447,#7448,#7449,#7450,#7451,#7452,#7453));
#1765=EDGE_LOOP('',(#7454,#7455,#7456,#7457));
#1766=EDGE_LOOP('',(#7458,#7459,#7460,#7461,#7462,#7463));
#1767=EDGE_LOOP('',(#7464,#7465,#7466,#7467,#7468,#7469));
#1768=EDGE_LOOP('',(#7470));
#1769=EDGE_LOOP('',(#7471));
#1770=EDGE_LOOP('',(#7472));
#1771=EDGE_LOOP('',(#7473));
#1772=EDGE_LOOP('',(#7474,#7475,#7476,#7477));
#1773=EDGE_LOOP('',(#7478,#7479,#7480,#7481));
#1774=EDGE_LOOP('',(#7482,#7483,#7484,#7485));
#1775=EDGE_LOOP('',(#7486,#7487,#7488,#7489));
#1776=EDGE_LOOP('',(#7490,#7491,#7492,#7493));
#1777=EDGE_LOOP('',(#7494,#7495,#7496,#7497));
#1778=EDGE_LOOP('',(#7498,#7499,#7500,#7501));
#1779=EDGE_LOOP('',(#7502,#7503,#7504,#7505));
#1780=EDGE_LOOP('',(#7506,#7507,#7508,#7509));
#1781=EDGE_LOOP('',(#7510,#7511,#7512,#7513));
#1782=EDGE_LOOP('',(#7514,#7515,#7516,#7517));
#1783=EDGE_LOOP('',(#7518,#7519,#7520,#7521));
#1784=EDGE_LOOP('',(#7522,#7523,#7524,#7525));
#1785=EDGE_LOOP('',(#7526,#7527,#7528,#7529));
#1786=EDGE_LOOP('',(#7530,#7531,#7532,#7533));
#1787=EDGE_LOOP('',(#7534,#7535,#7536,#7537));
#1788=EDGE_LOOP('',(#7538,#7539,#7540,#7541));
#1789=EDGE_LOOP('',(#7542,#7543,#7544,#7545));
#1790=EDGE_LOOP('',(#7546,#7547,#7548,#7549));
#1791=EDGE_LOOP('',(#7550,#7551,#7552,#7553));
#1792=EDGE_LOOP('',(#7554,#7555,#7556,#7557));
#1793=EDGE_LOOP('',(#7558,#7559,#7560,#7561));
#1794=EDGE_LOOP('',(#7562,#7563,#7564,#7565));
#1795=EDGE_LOOP('',(#7566,#7567,#7568,#7569));
#1796=EDGE_LOOP('',(#7570,#7571,#7572,#7573));
#1797=EDGE_LOOP('',(#7574,#7575,#7576,#7577));
#1798=EDGE_LOOP('',(#7578,#7579,#7580,#7581));
#1799=EDGE_LOOP('',(#7582,#7583,#7584,#7585));
#1800=EDGE_LOOP('',(#7586,#7587,#7588,#7589));
#1801=EDGE_LOOP('',(#7590,#7591,#7592,#7593));
#1802=EDGE_LOOP('',(#7594,#7595,#7596,#7597));
#1803=EDGE_LOOP('',(#7598,#7599,#7600,#7601));
#1804=EDGE_LOOP('',(#7602,#7603,#7604,#7605));
#1805=EDGE_LOOP('',(#7606,#7607,#7608,#7609));
#1806=EDGE_LOOP('',(#7610,#7611,#7612,#7613));
#1807=EDGE_LOOP('',(#7614,#7615,#7616,#7617));
#1808=EDGE_LOOP('',(#7618,#7619,#7620,#7621));
#1809=EDGE_LOOP('',(#7622,#7623,#7624,#7625));
#1810=EDGE_LOOP('',(#7626,#7627,#7628,#7629));
#1811=EDGE_LOOP('',(#7630,#7631,#7632,#7633));
#1812=EDGE_LOOP('',(#7634,#7635,#7636,#7637));
#1813=EDGE_LOOP('',(#7638,#7639,#7640,#7641));
#1814=EDGE_LOOP('',(#7642,#7643,#7644,#7645));
#1815=EDGE_LOOP('',(#7646,#7647,#7648,#7649));
#1816=EDGE_LOOP('',(#7650,#7651,#7652,#7653));
#1817=EDGE_LOOP('',(#7654,#7655,#7656,#7657));
#1818=EDGE_LOOP('',(#7658,#7659,#7660,#7661));
#1819=EDGE_LOOP('',(#7662,#7663,#7664,#7665));
#1820=EDGE_LOOP('',(#7666,#7667,#7668,#7669));
#1821=EDGE_LOOP('',(#7670,#7671,#7672,#7673));
#1822=EDGE_LOOP('',(#7674,#7675,#7676,#7677));
#1823=EDGE_LOOP('',(#7678,#7679,#7680,#7681));
#1824=EDGE_LOOP('',(#7682,#7683,#7684,#7685));
#1825=EDGE_LOOP('',(#7686,#7687,#7688,#7689));
#1826=EDGE_LOOP('',(#7690,#7691,#7692,#7693));
#1827=EDGE_LOOP('',(#7694,#7695,#7696,#7697));
#1828=EDGE_LOOP('',(#7698,#7699,#7700,#7701));
#1829=EDGE_LOOP('',(#7702,#7703,#7704,#7705));
#1830=EDGE_LOOP('',(#7706,#7707,#7708,#7709));
#1831=EDGE_LOOP('',(#7710,#7711,#7712,#7713));
#1832=EDGE_LOOP('',(#7714,#7715,#7716,#7717));
#1833=EDGE_LOOP('',(#7718,#7719,#7720,#7721));
#1834=EDGE_LOOP('',(#7722,#7723,#7724,#7725,#7726,#7727,#7728,#7729));
#1835=EDGE_LOOP('',(#7730,#7731,#7732,#7733,#7734,#7735,#7736,#7737,#7738,
#7739,#7740,#7741,#7742,#7743,#7744,#7745,#7746,#7747,#7748,#7749,#7750,
#7751,#7752,#7753,#7754,#7755,#7756,#7757,#7758,#7759,#7760,#7761,#7762,
#7763,#7764,#7765,#7766,#7767,#7768,#7769,#7770,#7771,#7772,#7773,#7774,
#7775,#7776,#7777,#7778,#7779,#7780,#7781,#7782,#7783,#7784,#7785,#7786,
#7787,#7788,#7789,#7790,#7791,#7792,#7793));
#1836=EDGE_LOOP('',(#7794,#7795,#7796,#7797));
#1837=EDGE_LOOP('',(#7798,#7799,#7800,#7801,#7802,#7803,#7804,#7805,#7806,
#7807,#7808,#7809,#7810,#7811,#7812,#7813,#7814,#7815,#7816,#7817,#7818,
#7819,#7820,#7821,#7822,#7823,#7824,#7825,#7826,#7827,#7828,#7829,#7830,
#7831,#7832,#7833,#7834,#7835,#7836,#7837,#7838,#7839,#7840,#7841,#7842,
#7843,#7844,#7845,#7846,#7847,#7848,#7849,#7850,#7851,#7852,#7853,#7854,
#7855,#7856,#7857,#7858,#7859,#7860,#7861,#7862));
#1838=EDGE_LOOP('',(#7863,#7864,#7865,#7866));
#1839=EDGE_LOOP('',(#7867,#7868,#7869,#7870));
#1840=EDGE_LOOP('',(#7871,#7872,#7873,#7874));
#1841=EDGE_LOOP('',(#7875,#7876,#7877,#7878));
#1842=EDGE_LOOP('',(#7879,#7880,#7881,#7882));
#1843=EDGE_LOOP('',(#7883,#7884,#7885,#7886));
#1844=EDGE_LOOP('',(#7887,#7888,#7889,#7890));
#1845=EDGE_LOOP('',(#7891,#7892,#7893,#7894,#7895,#7896));
#1846=EDGE_LOOP('',(#7897));
#1847=EDGE_LOOP('',(#7898,#7899,#7900,#7901));
#1848=EDGE_LOOP('',(#7902,#7903,#7904,#7905));
#1849=EDGE_LOOP('',(#7906));
#1850=EDGE_LOOP('',(#7907,#7908,#7909,#7910,#7911,#7912));
#1851=EDGE_LOOP('',(#7913));
#1852=EDGE_LOOP('',(#7914,#7915,#7916));
#1853=EDGE_LOOP('',(#7917,#7918,#7919,#7920,#7921));
#1854=EDGE_LOOP('',(#7922,#7923,#7924,#7925));
#1855=EDGE_LOOP('',(#7926,#7927,#7928,#7929));
#1856=EDGE_LOOP('',(#7930,#7931,#7932,#7933));
#1857=EDGE_LOOP('',(#7934,#7935,#7936,#7937));
#1858=EDGE_LOOP('',(#7938,#7939,#7940,#7941));
#1859=EDGE_LOOP('',(#7942,#7943,#7944,#7945));
#1860=EDGE_LOOP('',(#7946,#7947,#7948,#7949));
#1861=EDGE_LOOP('',(#7950,#7951,#7952,#7953));
#1862=EDGE_LOOP('',(#7954,#7955,#7956,#7957));
#1863=EDGE_LOOP('',(#7958,#7959,#7960,#7961,#7962,#7963,#7964,#7965,#7966,
#7967,#7968,#7969,#7970,#7971));
#1864=EDGE_LOOP('',(#7972,#7973,#7974,#7975,#7976,#7977,#7978,#7979,#7980,
#7981,#7982,#7983,#7984));
#1865=EDGE_LOOP('',(#7985,#7986,#7987,#7988,#7989,#7990));
#1866=EDGE_LOOP('',(#7991,#7992,#7993,#7994));
#1867=EDGE_LOOP('',(#7995,#7996,#7997,#7998));
#1868=EDGE_LOOP('',(#7999,#8000,#8001,#8002));
#1869=EDGE_LOOP('',(#8003,#8004,#8005,#8006));
#1870=EDGE_LOOP('',(#8007,#8008,#8009,#8010));
#1871=EDGE_LOOP('',(#8011,#8012,#8013,#8014));
#1872=EDGE_LOOP('',(#8015,#8016,#8017,#8018));
#1873=EDGE_LOOP('',(#8019,#8020,#8021,#8022));
#1874=EDGE_LOOP('',(#8023,#8024,#8025,#8026,#8027,#8028));
#1875=EDGE_LOOP('',(#8029,#8030,#8031,#8032,#8033));
#1876=EDGE_LOOP('',(#8034,#8035,#8036,#8037));
#1877=EDGE_LOOP('',(#8038,#8039,#8040,#8041));
#1878=EDGE_LOOP('',(#8042));
#1879=EDGE_LOOP('',(#8043));
#1880=EDGE_LOOP('',(#8044,#8045,#8046,#8047));
#1881=EDGE_LOOP('',(#8048));
#1882=EDGE_LOOP('',(#8049));
#1883=EDGE_LOOP('',(#8050));
#1884=EDGE_LOOP('',(#8051,#8052,#8053,#8054));
#1885=EDGE_LOOP('',(#8055));
#1886=EDGE_LOOP('',(#8056));
#1887=EDGE_LOOP('',(#8057));
#1888=EDGE_LOOP('',(#8058,#8059,#8060,#8061));
#1889=EDGE_LOOP('',(#8062));
#1890=EDGE_LOOP('',(#8063));
#1891=EDGE_LOOP('',(#8064));
#1892=EDGE_LOOP('',(#8065,#8066,#8067,#8068));
#1893=EDGE_LOOP('',(#8069));
#1894=EDGE_LOOP('',(#8070,#8071,#8072,#8073));
#1895=EDGE_LOOP('',(#8074,#8075,#8076,#8077));
#1896=EDGE_LOOP('',(#8078,#8079,#8080,#8081));
#1897=EDGE_LOOP('',(#8082,#8083,#8084,#8085));
#1898=EDGE_LOOP('',(#8086,#8087,#8088,#8089));
#1899=EDGE_LOOP('',(#8090,#8091,#8092,#8093));
#1900=EDGE_LOOP('',(#8094,#8095,#8096,#8097));
#1901=EDGE_LOOP('',(#8098,#8099,#8100,#8101));
#1902=EDGE_LOOP('',(#8102,#8103,#8104,#8105));
#1903=EDGE_LOOP('',(#8106,#8107,#8108,#8109));
#1904=EDGE_LOOP('',(#8110,#8111,#8112,#8113));
#1905=EDGE_LOOP('',(#8114,#8115,#8116,#8117));
#1906=EDGE_LOOP('',(#8118,#8119,#8120,#8121));
#1907=EDGE_LOOP('',(#8122,#8123,#8124,#8125));
#1908=EDGE_LOOP('',(#8126,#8127,#8128,#8129));
#1909=EDGE_LOOP('',(#8130,#8131,#8132,#8133));
#1910=EDGE_LOOP('',(#8134,#8135,#8136,#8137,#8138,#8139,#8140,#8141));
#1911=EDGE_LOOP('',(#8142));
#1912=EDGE_LOOP('',(#8143));
#1913=EDGE_LOOP('',(#8144,#8145,#8146,#8147));
#1914=EDGE_LOOP('',(#8148,#8149,#8150,#8151));
#1915=EDGE_LOOP('',(#8152,#8153,#8154,#8155));
#1916=EDGE_LOOP('',(#8156,#8157,#8158,#8159,#8160,#8161,#8162,#8163));
#1917=EDGE_LOOP('',(#8164));
#1918=EDGE_LOOP('',(#8165));
#1919=EDGE_LOOP('',(#8166));
#1920=EDGE_LOOP('',(#8167));
#1921=EDGE_LOOP('',(#8168));
#1922=EDGE_LOOP('',(#8169));
#1923=EDGE_LOOP('',(#8170,#8171,#8172,#8173));
#1924=EDGE_LOOP('',(#8174,#8175,#8176,#8177));
#1925=EDGE_LOOP('',(#8178,#8179,#8180,#8181));
#1926=EDGE_LOOP('',(#8182));
#1927=EDGE_LOOP('',(#8183));
#1928=EDGE_LOOP('',(#8184));
#1929=EDGE_LOOP('',(#8185));
#1930=LINE('',#11412,#2660);
#1931=LINE('',#11418,#2661);
#1932=LINE('',#11424,#2662);
#1933=LINE('',#11429,#2663);
#1934=LINE('',#11431,#2664);
#1935=LINE('',#11433,#2665);
#1936=LINE('',#11434,#2666);
#1937=LINE('',#11438,#2667);
#1938=LINE('',#11439,#2668);
#1939=LINE('',#11440,#2669);
#1940=LINE('',#11444,#2670);
#1941=LINE('',#11446,#2671);
#1942=LINE('',#11448,#2672);
#1943=LINE('',#11449,#2673);
#1944=LINE('',#11453,#2674);
#1945=LINE('',#11454,#2675);
#1946=LINE('',#11455,#2676);
#1947=LINE('',#11459,#2677);
#1948=LINE('',#11461,#2678);
#1949=LINE('',#11463,#2679);
#1950=LINE('',#11464,#2680);
#1951=LINE('',#11468,#2681);
#1952=LINE('',#11469,#2682);
#1953=LINE('',#11470,#2683);
#1954=LINE('',#11474,#2684);
#1955=LINE('',#11476,#2685);
#1956=LINE('',#11478,#2686);
#1957=LINE('',#11479,#2687);
#1958=LINE('',#11483,#2688);
#1959=LINE('',#11484,#2689);
#1960=LINE('',#11485,#2690);
#1961=LINE('',#11489,#2691);
#1962=LINE('',#11491,#2692);
#1963=LINE('',#11493,#2693);
#1964=LINE('',#11494,#2694);
#1965=LINE('',#11498,#2695);
#1966=LINE('',#11499,#2696);
#1967=LINE('',#11500,#2697);
#1968=LINE('',#11504,#2698);
#1969=LINE('',#11506,#2699);
#1970=LINE('',#11508,#2700);
#1971=LINE('',#11509,#2701);
#1972=LINE('',#11513,#2702);
#1973=LINE('',#11514,#2703);
#1974=LINE('',#11515,#2704);
#1975=LINE('',#11519,#2705);
#1976=LINE('',#11521,#2706);
#1977=LINE('',#11523,#2707);
#1978=LINE('',#11524,#2708);
#1979=LINE('',#11528,#2709);
#1980=LINE('',#11529,#2710);
#1981=LINE('',#11530,#2711);
#1982=LINE('',#11534,#2712);
#1983=LINE('',#11536,#2713);
#1984=LINE('',#11538,#2714);
#1985=LINE('',#11539,#2715);
#1986=LINE('',#11543,#2716);
#1987=LINE('',#11544,#2717);
#1988=LINE('',#11545,#2718);
#1989=LINE('',#11549,#2719);
#1990=LINE('',#11551,#2720);
#1991=LINE('',#11553,#2721);
#1992=LINE('',#11554,#2722);
#1993=LINE('',#11558,#2723);
#1994=LINE('',#11559,#2724);
#1995=LINE('',#11560,#2725);
#1996=LINE('',#11564,#2726);
#1997=LINE('',#11566,#2727);
#1998=LINE('',#11568,#2728);
#1999=LINE('',#11569,#2729);
#2000=LINE('',#11573,#2730);
#2001=LINE('',#11574,#2731);
#2002=LINE('',#11575,#2732);
#2003=LINE('',#11579,#2733);
#2004=LINE('',#11581,#2734);
#2005=LINE('',#11583,#2735);
#2006=LINE('',#11584,#2736);
#2007=LINE('',#11588,#2737);
#2008=LINE('',#11589,#2738);
#2009=LINE('',#11590,#2739);
#2010=LINE('',#11594,#2740);
#2011=LINE('',#11596,#2741);
#2012=LINE('',#11598,#2742);
#2013=LINE('',#11599,#2743);
#2014=LINE('',#11603,#2744);
#2015=LINE('',#11604,#2745);
#2016=LINE('',#11605,#2746);
#2017=LINE('',#11609,#2747);
#2018=LINE('',#11611,#2748);
#2019=LINE('',#11613,#2749);
#2020=LINE('',#11614,#2750);
#2021=LINE('',#11618,#2751);
#2022=LINE('',#11619,#2752);
#2023=LINE('',#11620,#2753);
#2024=LINE('',#11624,#2754);
#2025=LINE('',#11626,#2755);
#2026=LINE('',#11628,#2756);
#2027=LINE('',#11629,#2757);
#2028=LINE('',#11633,#2758);
#2029=LINE('',#11634,#2759);
#2030=LINE('',#11635,#2760);
#2031=LINE('',#11639,#2761);
#2032=LINE('',#11641,#2762);
#2033=LINE('',#11643,#2763);
#2034=LINE('',#11644,#2764);
#2035=LINE('',#11648,#2765);
#2036=LINE('',#11649,#2766);
#2037=LINE('',#11650,#2767);
#2038=LINE('',#11654,#2768);
#2039=LINE('',#11656,#2769);
#2040=LINE('',#11658,#2770);
#2041=LINE('',#11659,#2771);
#2042=LINE('',#11663,#2772);
#2043=LINE('',#11664,#2773);
#2044=LINE('',#11665,#2774);
#2045=LINE('',#11669,#2775);
#2046=LINE('',#11671,#2776);
#2047=LINE('',#11673,#2777);
#2048=LINE('',#11674,#2778);
#2049=LINE('',#11678,#2779);
#2050=LINE('',#11679,#2780);
#2051=LINE('',#11680,#2781);
#2052=LINE('',#11684,#2782);
#2053=LINE('',#11686,#2783);
#2054=LINE('',#11688,#2784);
#2055=LINE('',#11689,#2785);
#2056=LINE('',#11693,#2786);
#2057=LINE('',#11694,#2787);
#2058=LINE('',#11695,#2788);
#2059=LINE('',#11699,#2789);
#2060=LINE('',#11701,#2790);
#2061=LINE('',#11703,#2791);
#2062=LINE('',#11704,#2792);
#2063=LINE('',#11708,#2793);
#2064=LINE('',#11709,#2794);
#2065=LINE('',#11710,#2795);
#2066=LINE('',#11714,#2796);
#2067=LINE('',#11716,#2797);
#2068=LINE('',#11718,#2798);
#2069=LINE('',#11719,#2799);
#2070=LINE('',#11723,#2800);
#2071=LINE('',#11724,#2801);
#2072=LINE('',#11725,#2802);
#2073=LINE('',#11729,#2803);
#2074=LINE('',#11731,#2804);
#2075=LINE('',#11733,#2805);
#2076=LINE('',#11734,#2806);
#2077=LINE('',#11738,#2807);
#2078=LINE('',#11739,#2808);
#2079=LINE('',#11740,#2809);
#2080=LINE('',#11744,#2810);
#2081=LINE('',#11746,#2811);
#2082=LINE('',#11748,#2812);
#2083=LINE('',#11749,#2813);
#2084=LINE('',#11753,#2814);
#2085=LINE('',#11754,#2815);
#2086=LINE('',#11755,#2816);
#2087=LINE('',#11759,#2817);
#2088=LINE('',#11761,#2818);
#2089=LINE('',#11763,#2819);
#2090=LINE('',#11764,#2820);
#2091=LINE('',#11768,#2821);
#2092=LINE('',#11769,#2822);
#2093=LINE('',#11770,#2823);
#2094=LINE('',#11774,#2824);
#2095=LINE('',#11776,#2825);
#2096=LINE('',#11778,#2826);
#2097=LINE('',#11779,#2827);
#2098=LINE('',#11783,#2828);
#2099=LINE('',#11784,#2829);
#2100=LINE('',#11785,#2830);
#2101=LINE('',#11789,#2831);
#2102=LINE('',#11791,#2832);
#2103=LINE('',#11793,#2833);
#2104=LINE('',#11794,#2834);
#2105=LINE('',#11798,#2835);
#2106=LINE('',#11799,#2836);
#2107=LINE('',#11800,#2837);
#2108=LINE('',#11804,#2838);
#2109=LINE('',#11806,#2839);
#2110=LINE('',#11808,#2840);
#2111=LINE('',#11809,#2841);
#2112=LINE('',#11813,#2842);
#2113=LINE('',#11814,#2843);
#2114=LINE('',#11815,#2844);
#2115=LINE('',#11819,#2845);
#2116=LINE('',#11821,#2846);
#2117=LINE('',#11823,#2847);
#2118=LINE('',#11824,#2848);
#2119=LINE('',#11828,#2849);
#2120=LINE('',#11829,#2850);
#2121=LINE('',#11830,#2851);
#2122=LINE('',#11834,#2852);
#2123=LINE('',#11836,#2853);
#2124=LINE('',#11838,#2854);
#2125=LINE('',#11839,#2855);
#2126=LINE('',#11843,#2856);
#2127=LINE('',#11844,#2857);
#2128=LINE('',#11845,#2858);
#2129=LINE('',#11849,#2859);
#2130=LINE('',#11851,#2860);
#2131=LINE('',#11853,#2861);
#2132=LINE('',#11854,#2862);
#2133=LINE('',#11858,#2863);
#2134=LINE('',#11859,#2864);
#2135=LINE('',#11860,#2865);
#2136=LINE('',#11864,#2866);
#2137=LINE('',#11866,#2867);
#2138=LINE('',#11868,#2868);
#2139=LINE('',#11869,#2869);
#2140=LINE('',#11873,#2870);
#2141=LINE('',#11874,#2871);
#2142=LINE('',#11875,#2872);
#2143=LINE('',#11879,#2873);
#2144=LINE('',#11881,#2874);
#2145=LINE('',#11883,#2875);
#2146=LINE('',#11884,#2876);
#2147=LINE('',#11888,#2877);
#2148=LINE('',#11889,#2878);
#2149=LINE('',#11890,#2879);
#2150=LINE('',#11894,#2880);
#2151=LINE('',#11896,#2881);
#2152=LINE('',#11898,#2882);
#2153=LINE('',#11899,#2883);
#2154=LINE('',#11903,#2884);
#2155=LINE('',#11904,#2885);
#2156=LINE('',#11905,#2886);
#2157=LINE('',#11909,#2887);
#2158=LINE('',#11911,#2888);
#2159=LINE('',#11913,#2889);
#2160=LINE('',#11914,#2890);
#2161=LINE('',#11918,#2891);
#2162=LINE('',#11919,#2892);
#2163=LINE('',#11920,#2893);
#2164=LINE('',#11924,#2894);
#2165=LINE('',#11926,#2895);
#2166=LINE('',#11928,#2896);
#2167=LINE('',#11929,#2897);
#2168=LINE('',#11933,#2898);
#2169=LINE('',#11934,#2899);
#2170=LINE('',#11935,#2900);
#2171=LINE('',#11939,#2901);
#2172=LINE('',#11941,#2902);
#2173=LINE('',#11943,#2903);
#2174=LINE('',#11944,#2904);
#2175=LINE('',#11948,#2905);
#2176=LINE('',#11949,#2906);
#2177=LINE('',#11950,#2907);
#2178=LINE('',#11954,#2908);
#2179=LINE('',#11956,#2909);
#2180=LINE('',#11958,#2910);
#2181=LINE('',#11959,#2911);
#2182=LINE('',#11963,#2912);
#2183=LINE('',#11964,#2913);
#2184=LINE('',#11965,#2914);
#2185=LINE('',#11969,#2915);
#2186=LINE('',#11971,#2916);
#2187=LINE('',#11973,#2917);
#2188=LINE('',#11974,#2918);
#2189=LINE('',#11978,#2919);
#2190=LINE('',#11979,#2920);
#2191=LINE('',#11980,#2921);
#2192=LINE('',#11984,#2922);
#2193=LINE('',#11986,#2923);
#2194=LINE('',#11988,#2924);
#2195=LINE('',#11989,#2925);
#2196=LINE('',#11993,#2926);
#2197=LINE('',#11994,#2927);
#2198=LINE('',#11995,#2928);
#2199=LINE('',#11998,#2929);
#2200=LINE('',#12000,#2930);
#2201=LINE('',#12002,#2931);
#2202=LINE('',#12004,#2932);
#2203=LINE('',#12005,#2933);
#2204=LINE('',#12007,#2934);
#2205=LINE('',#12008,#2935);
#2206=LINE('',#12010,#2936);
#2207=LINE('',#12011,#2937);
#2208=LINE('',#12013,#2938);
#2209=LINE('',#12014,#2939);
#2210=LINE('',#12016,#2940);
#2211=LINE('',#12017,#2941);
#2212=LINE('',#12019,#2942);
#2213=LINE('',#12020,#2943);
#2214=LINE('',#12022,#2944);
#2215=LINE('',#12023,#2945);
#2216=LINE('',#12025,#2946);
#2217=LINE('',#12026,#2947);
#2218=LINE('',#12028,#2948);
#2219=LINE('',#12029,#2949);
#2220=LINE('',#12031,#2950);
#2221=LINE('',#12032,#2951);
#2222=LINE('',#12034,#2952);
#2223=LINE('',#12035,#2953);
#2224=LINE('',#12037,#2954);
#2225=LINE('',#12038,#2955);
#2226=LINE('',#12040,#2956);
#2227=LINE('',#12041,#2957);
#2228=LINE('',#12043,#2958);
#2229=LINE('',#12044,#2959);
#2230=LINE('',#12046,#2960);
#2231=LINE('',#12047,#2961);
#2232=LINE('',#12049,#2962);
#2233=LINE('',#12050,#2963);
#2234=LINE('',#12052,#2964);
#2235=LINE('',#12053,#2965);
#2236=LINE('',#12055,#2966);
#2237=LINE('',#12056,#2967);
#2238=LINE('',#12058,#2968);
#2239=LINE('',#12059,#2969);
#2240=LINE('',#12061,#2970);
#2241=LINE('',#12062,#2971);
#2242=LINE('',#12064,#2972);
#2243=LINE('',#12065,#2973);
#2244=LINE('',#12067,#2974);
#2245=LINE('',#12068,#2975);
#2246=LINE('',#12070,#2976);
#2247=LINE('',#12071,#2977);
#2248=LINE('',#12073,#2978);
#2249=LINE('',#12074,#2979);
#2250=LINE('',#12076,#2980);
#2251=LINE('',#12077,#2981);
#2252=LINE('',#12079,#2982);
#2253=LINE('',#12080,#2983);
#2254=LINE('',#12082,#2984);
#2255=LINE('',#12083,#2985);
#2256=LINE('',#12085,#2986);
#2257=LINE('',#12086,#2987);
#2258=LINE('',#12088,#2988);
#2259=LINE('',#12089,#2989);
#2260=LINE('',#12092,#2990);
#2261=LINE('',#12094,#2991);
#2262=LINE('',#12095,#2992);
#2263=LINE('',#12097,#2993);
#2264=LINE('',#12098,#2994);
#2265=LINE('',#12100,#2995);
#2266=LINE('',#12101,#2996);
#2267=LINE('',#12103,#2997);
#2268=LINE('',#12104,#2998);
#2269=LINE('',#12106,#2999);
#2270=LINE('',#12107,#3000);
#2271=LINE('',#12109,#3001);
#2272=LINE('',#12110,#3002);
#2273=LINE('',#12112,#3003);
#2274=LINE('',#12113,#3004);
#2275=LINE('',#12115,#3005);
#2276=LINE('',#12116,#3006);
#2277=LINE('',#12118,#3007);
#2278=LINE('',#12119,#3008);
#2279=LINE('',#12121,#3009);
#2280=LINE('',#12122,#3010);
#2281=LINE('',#12125,#3011);
#2282=LINE('',#12127,#3012);
#2283=LINE('',#12129,#3013);
#2284=LINE('',#12130,#3014);
#2285=LINE('',#12133,#3015);
#2286=LINE('',#12134,#3016);
#2287=LINE('',#12138,#3017);
#2288=LINE('',#12140,#3018);
#2289=LINE('',#12142,#3019);
#2290=LINE('',#12143,#3020);
#2291=LINE('',#12146,#3021);
#2292=LINE('',#12147,#3022);
#2293=LINE('',#12150,#3023);
#2294=LINE('',#12151,#3024);
#2295=LINE('',#12153,#3025);
#2296=LINE('',#12154,#3026);
#2297=LINE('',#12159,#3027);
#2298=LINE('',#12161,#3028);
#2299=LINE('',#12163,#3029);
#2300=LINE('',#12165,#3030);
#2301=LINE('',#12167,#3031);
#2302=LINE('',#12169,#3032);
#2303=LINE('',#12174,#3033);
#2304=LINE('',#12177,#3034);
#2305=LINE('',#12179,#3035);
#2306=LINE('',#12180,#3036);
#2307=LINE('',#12183,#3037);
#2308=LINE('',#12184,#3038);
#2309=LINE('',#12187,#3039);
#2310=LINE('',#12188,#3040);
#2311=LINE('',#12191,#3041);
#2312=LINE('',#12192,#3042);
#2313=LINE('',#12195,#3043);
#2314=LINE('',#12196,#3044);
#2315=LINE('',#12198,#3045);
#2316=LINE('',#12207,#3046);
#2317=LINE('',#12218,#3047);
#2318=LINE('',#12226,#3048);
#2319=LINE('',#12230,#3049);
#2320=LINE('',#12236,#3050);
#2321=LINE('',#12238,#3051);
#2322=LINE('',#12240,#3052);
#2323=LINE('',#12241,#3053);
#2324=LINE('',#12245,#3054);
#2325=LINE('',#12247,#3055);
#2326=LINE('',#12249,#3056);
#2327=LINE('',#12250,#3057);
#2328=LINE('',#12555,#3058);
#2329=LINE('',#12557,#3059);
#2330=LINE('',#12571,#3060);
#2331=LINE('',#12576,#3061);
#2332=LINE('',#12582,#3062);
#2333=LINE('',#12587,#3063);
#2334=LINE('',#12592,#3064);
#2335=LINE('',#12601,#3065);
#2336=LINE('',#12608,#3066);
#2337=LINE('',#12612,#3067);
#2338=LINE('',#12617,#3068);
#2339=LINE('',#12619,#3069);
#2340=LINE('',#12621,#3070);
#2341=LINE('',#12622,#3071);
#2342=LINE('',#12626,#3072);
#2343=LINE('',#12628,#3073);
#2344=LINE('',#12630,#3074);
#2345=LINE('',#12631,#3075);
#2346=LINE('',#12635,#3076);
#2347=LINE('',#12637,#3077);
#2348=LINE('',#12639,#3078);
#2349=LINE('',#12640,#3079);
#2350=LINE('',#12644,#3080);
#2351=LINE('',#12646,#3081);
#2352=LINE('',#12648,#3082);
#2353=LINE('',#12649,#3083);
#2354=LINE('',#12653,#3084);
#2355=LINE('',#12655,#3085);
#2356=LINE('',#12657,#3086);
#2357=LINE('',#12658,#3087);
#2358=LINE('',#12662,#3088);
#2359=LINE('',#12664,#3089);
#2360=LINE('',#12666,#3090);
#2361=LINE('',#12667,#3091);
#2362=LINE('',#12671,#3092);
#2363=LINE('',#12673,#3093);
#2364=LINE('',#12675,#3094);
#2365=LINE('',#12676,#3095);
#2366=LINE('',#12684,#3096);
#2367=LINE('',#12685,#3097);
#2368=LINE('',#12687,#3098);
#2369=LINE('',#12688,#3099);
#2370=LINE('',#12690,#3100);
#2371=LINE('',#12691,#3101);
#2372=LINE('',#12694,#3102);
#2373=LINE('',#12696,#3103);
#2374=LINE('',#12697,#3104);
#2375=LINE('',#12700,#3105);
#2376=LINE('',#12702,#3106);
#2377=LINE('',#12703,#3107);
#2378=LINE('',#12707,#3108);
#2379=LINE('',#12751,#3109);
#2380=LINE('',#12794,#3110);
#2381=LINE('',#12797,#3111);
#2382=LINE('',#12835,#3112);
#2383=LINE('',#12872,#3113);
#2384=LINE('',#12875,#3114);
#2385=LINE('',#12883,#3115);
#2386=LINE('',#12920,#3116);
#2387=LINE('',#12923,#3117);
#2388=LINE('',#12930,#3118);
#2389=LINE('',#12936,#3119);
#2390=LINE('',#12947,#3120);
#2391=LINE('',#12956,#3121);
#2392=LINE('',#12962,#3122);
#2393=LINE('',#12997,#3123);
#2394=LINE('',#13068,#3124);
#2395=LINE('',#13138,#3125);
#2396=LINE('',#13170,#3126);
#2397=LINE('',#13176,#3127);
#2398=LINE('',#13185,#3128);
#2399=LINE('',#13222,#3129);
#2400=LINE('',#13257,#3130);
#2401=LINE('',#13259,#3131);
#2402=LINE('',#13263,#3132);
#2403=LINE('',#13309,#3133);
#2404=LINE('',#13435,#3134);
#2405=LINE('',#13515,#3135);
#2406=LINE('',#13677,#3136);
#2407=LINE('',#13787,#3137);
#2408=LINE('',#13876,#3138);
#2409=LINE('',#13964,#3139);
#2410=LINE('',#14076,#3140);
#2411=LINE('',#14077,#3141);
#2412=LINE('',#14114,#3142);
#2413=LINE('',#14115,#3143);
#2414=LINE('',#14600,#3144);
#2415=LINE('',#14602,#3145);
#2416=LINE('',#14616,#3146);
#2417=LINE('',#14618,#3147);
#2418=LINE('',#14620,#3148);
#2419=LINE('',#14621,#3149);
#2420=LINE('',#14624,#3150);
#2421=LINE('',#14626,#3151);
#2422=LINE('',#14627,#3152);
#2423=LINE('',#14630,#3153);
#2424=LINE('',#14632,#3154);
#2425=LINE('',#14633,#3155);
#2426=LINE('',#14636,#3156);
#2427=LINE('',#14638,#3157);
#2428=LINE('',#14639,#3158);
#2429=LINE('',#14642,#3159);
#2430=LINE('',#14644,#3160);
#2431=LINE('',#14645,#3161);
#2432=LINE('',#14647,#3162);
#2433=LINE('',#14648,#3163);
#2434=LINE('',#14655,#3164);
#2435=LINE('',#14657,#3165);
#2436=LINE('',#14659,#3166);
#2437=LINE('',#14660,#3167);
#2438=LINE('',#14663,#3168);
#2439=LINE('',#14665,#3169);
#2440=LINE('',#14666,#3170);
#2441=LINE('',#14669,#3171);
#2442=LINE('',#14671,#3172);
#2443=LINE('',#14672,#3173);
#2444=LINE('',#14675,#3174);
#2445=LINE('',#14677,#3175);
#2446=LINE('',#14678,#3176);
#2447=LINE('',#14681,#3177);
#2448=LINE('',#14683,#3178);
#2449=LINE('',#14684,#3179);
#2450=LINE('',#14686,#3180);
#2451=LINE('',#14687,#3181);
#2452=LINE('',#14694,#3182);
#2453=LINE('',#14699,#3183);
#2454=LINE('',#14705,#3184);
#2455=LINE('',#14710,#3185);
#2456=LINE('',#14713,#3186);
#2457=LINE('',#14717,#3187);
#2458=LINE('',#14722,#3188);
#2459=LINE('',#14724,#3189);
#2460=LINE('',#14726,#3190);
#2461=LINE('',#14727,#3191);
#2462=LINE('',#14731,#3192);
#2463=LINE('',#14733,#3193);
#2464=LINE('',#14735,#3194);
#2465=LINE('',#14736,#3195);
#2466=LINE('',#14740,#3196);
#2467=LINE('',#14742,#3197);
#2468=LINE('',#14744,#3198);
#2469=LINE('',#14745,#3199);
#2470=LINE('',#14749,#3200);
#2471=LINE('',#14751,#3201);
#2472=LINE('',#14753,#3202);
#2473=LINE('',#14754,#3203);
#2474=LINE('',#14758,#3204);
#2475=LINE('',#14760,#3205);
#2476=LINE('',#14762,#3206);
#2477=LINE('',#14763,#3207);
#2478=LINE('',#14767,#3208);
#2479=LINE('',#14769,#3209);
#2480=LINE('',#14771,#3210);
#2481=LINE('',#14772,#3211);
#2482=LINE('',#14776,#3212);
#2483=LINE('',#14778,#3213);
#2484=LINE('',#14780,#3214);
#2485=LINE('',#14781,#3215);
#2486=LINE('',#14789,#3216);
#2487=LINE('',#14790,#3217);
#2488=LINE('',#14792,#3218);
#2489=LINE('',#14793,#3219);
#2490=LINE('',#14795,#3220);
#2491=LINE('',#14796,#3221);
#2492=LINE('',#14799,#3222);
#2493=LINE('',#14801,#3223);
#2494=LINE('',#14802,#3224);
#2495=LINE('',#14805,#3225);
#2496=LINE('',#14807,#3226);
#2497=LINE('',#14808,#3227);
#2498=LINE('',#14812,#3228);
#2499=LINE('',#14856,#3229);
#2500=LINE('',#14899,#3230);
#2501=LINE('',#14902,#3231);
#2502=LINE('',#14940,#3232);
#2503=LINE('',#14977,#3233);
#2504=LINE('',#14980,#3234);
#2505=LINE('',#14988,#3235);
#2506=LINE('',#15025,#3236);
#2507=LINE('',#15028,#3237);
#2508=LINE('',#15035,#3238);
#2509=LINE('',#15041,#3239);
#2510=LINE('',#15052,#3240);
#2511=LINE('',#15061,#3241);
#2512=LINE('',#15067,#3242);
#2513=LINE('',#15102,#3243);
#2514=LINE('',#15173,#3244);
#2515=LINE('',#15243,#3245);
#2516=LINE('',#15275,#3246);
#2517=LINE('',#15281,#3247);
#2518=LINE('',#15290,#3248);
#2519=LINE('',#15327,#3249);
#2520=LINE('',#15362,#3250);
#2521=LINE('',#15364,#3251);
#2522=LINE('',#15368,#3252);
#2523=LINE('',#15414,#3253);
#2524=LINE('',#15540,#3254);
#2525=LINE('',#15620,#3255);
#2526=LINE('',#15782,#3256);
#2527=LINE('',#15892,#3257);
#2528=LINE('',#15981,#3258);
#2529=LINE('',#16069,#3259);
#2530=LINE('',#16181,#3260);
#2531=LINE('',#16182,#3261);
#2532=LINE('',#16219,#3262);
#2533=LINE('',#16220,#3263);
#2534=LINE('',#16414,#3264);
#2535=LINE('',#16438,#3265);
#2536=LINE('',#16486,#3266);
#2537=LINE('',#16534,#3267);
#2538=LINE('',#16585,#3268);
#2539=LINE('',#16633,#3269);
#2540=LINE('',#16681,#3270);
#2541=LINE('',#16729,#3271);
#2542=LINE('',#16783,#3272);
#2543=LINE('',#16831,#3273);
#2544=LINE('',#16879,#3274);
#2545=LINE('',#16933,#3275);
#2546=LINE('',#16981,#3276);
#2547=LINE('',#17029,#3277);
#2548=LINE('',#17077,#3278);
#2549=LINE('',#17131,#3279);
#2550=LINE('',#17179,#3280);
#2551=LINE('',#17227,#3281);
#2552=LINE('',#17281,#3282);
#2553=LINE('',#17329,#3283);
#2554=LINE('',#17377,#3284);
#2555=LINE('',#17431,#3285);
#2556=LINE('',#17479,#3286);
#2557=LINE('',#17527,#3287);
#2558=LINE('',#17575,#3288);
#2559=LINE('',#17629,#3289);
#2560=LINE('',#17677,#3290);
#2561=LINE('',#17725,#3291);
#2562=LINE('',#17779,#3292);
#2563=LINE('',#17827,#3293);
#2564=LINE('',#17875,#3294);
#2565=LINE('',#17901,#3295);
#2566=LINE('',#17925,#3296);
#2567=LINE('',#17949,#3297);
#2568=LINE('',#17974,#3298);
#2569=LINE('',#17999,#3299);
#2570=LINE('',#18023,#3300);
#2571=LINE('',#18048,#3301);
#2572=LINE('',#18073,#3302);
#2573=LINE('',#18097,#3303);
#2574=LINE('',#18121,#3304);
#2575=LINE('',#18146,#3305);
#2576=LINE('',#18171,#3306);
#2577=LINE('',#18195,#3307);
#2578=LINE('',#18220,#3308);
#2579=LINE('',#18245,#3309);
#2580=LINE('',#18269,#3310);
#2581=LINE('',#18294,#3311);
#2582=LINE('',#18319,#3312);
#2583=LINE('',#18343,#3313);
#2584=LINE('',#18367,#3314);
#2585=LINE('',#18392,#3315);
#2586=LINE('',#18417,#3316);
#2587=LINE('',#18441,#3317);
#2588=LINE('',#18466,#3318);
#2589=LINE('',#18491,#3319);
#2590=LINE('',#18515,#3320);
#2591=LINE('',#18540,#3321);
#2592=LINE('',#18564,#3322);
#2593=LINE('',#18589,#3323);
#2594=LINE('',#18790,#3324);
#2595=LINE('',#20535,#3325);
#2596=LINE('',#20537,#3326);
#2597=LINE('',#20539,#3327);
#2598=LINE('',#20540,#3328);
#2599=LINE('',#20543,#3329);
#2600=LINE('',#20545,#3330);
#2601=LINE('',#20546,#3331);
#2602=LINE('',#20549,#3332);
#2603=LINE('',#20551,#3333);
#2604=LINE('',#20552,#3334);
#2605=LINE('',#20555,#3335);
#2606=LINE('',#20557,#3336);
#2607=LINE('',#20558,#3337);
#2608=LINE('',#20561,#3338);
#2609=LINE('',#20563,#3339);
#2610=LINE('',#20564,#3340);
#2611=LINE('',#20566,#3341);
#2612=LINE('',#20567,#3342);
#2613=LINE('',#20574,#3343);
#2614=LINE('',#20582,#3344);
#2615=LINE('',#20595,#3345);
#2616=LINE('',#20642,#3346);
#2617=LINE('',#20696,#3347);
#2618=LINE('',#20744,#3348);
#2619=LINE('',#20783,#3349);
#2620=LINE('',#20804,#3350);
#2621=LINE('',#20829,#3351);
#2622=LINE('',#20854,#3352);
#2623=LINE('',#20879,#3353);
#2624=LINE('',#21452,#3354);
#2625=LINE('',#21454,#3355);
#2626=LINE('',#21456,#3356);
#2627=LINE('',#21458,#3357);
#2628=LINE('',#21460,#3358);
#2629=LINE('',#21461,#3359);
#2630=LINE('',#21466,#3360);
#2631=LINE('',#21467,#3361);
#2632=LINE('',#21468,#3362);
#2633=LINE('',#21471,#3363);
#2634=LINE('',#21472,#3364);
#2635=LINE('',#21475,#3365);
#2636=LINE('',#21476,#3366);
#2637=LINE('',#21479,#3367);
#2638=LINE('',#21480,#3368);
#2639=LINE('',#21483,#3369);
#2640=LINE('',#21484,#3370);
#2641=LINE('',#21486,#3371);
#2642=LINE('',#21493,#3372);
#2643=LINE('',#21499,#3373);
#2644=LINE('',#21509,#3374);
#2645=LINE('',#21519,#3375);
#2646=LINE('',#21529,#3376);
#2647=LINE('',#21539,#3377);
#2648=LINE('',#21543,#3378);
#2649=LINE('',#21547,#3379);
#2650=LINE('',#21551,#3380);
#2651=LINE('',#21555,#3381);
#2652=LINE('',#21602,#3382);
#2653=LINE('',#21603,#3383);
#2654=LINE('',#21722,#3384);
#2655=LINE('',#21723,#3385);
#2656=LINE('',#21804,#3386);
#2657=LINE('',#21947,#3387);
#2658=LINE('',#22088,#3388);
#2659=LINE('',#22094,#3389);
#2660=VECTOR('',#9508,0.17);
#2661=VECTOR('',#9515,0.17);
#2662=VECTOR('',#9522,0.41);
#2663=VECTOR('',#9527,1.);
#2664=VECTOR('',#9528,1.);
#2665=VECTOR('',#9529,1.);
#2666=VECTOR('',#9530,1.);
#2667=VECTOR('',#9533,1.);
#2668=VECTOR('',#9534,1.);
#2669=VECTOR('',#9535,1.);
#2670=VECTOR('',#9538,1.);
#2671=VECTOR('',#9539,1.);
#2672=VECTOR('',#9540,1.);
#2673=VECTOR('',#9541,1.);
#2674=VECTOR('',#9544,1.);
#2675=VECTOR('',#9545,1.);
#2676=VECTOR('',#9546,1.);
#2677=VECTOR('',#9549,1.);
#2678=VECTOR('',#9550,1.);
#2679=VECTOR('',#9551,1.);
#2680=VECTOR('',#9552,1.);
#2681=VECTOR('',#9555,1.);
#2682=VECTOR('',#9556,1.);
#2683=VECTOR('',#9557,1.);
#2684=VECTOR('',#9560,1.);
#2685=VECTOR('',#9561,1.);
#2686=VECTOR('',#9562,1.);
#2687=VECTOR('',#9563,1.);
#2688=VECTOR('',#9566,1.);
#2689=VECTOR('',#9567,1.);
#2690=VECTOR('',#9568,1.);
#2691=VECTOR('',#9571,1.);
#2692=VECTOR('',#9572,1.);
#2693=VECTOR('',#9573,1.);
#2694=VECTOR('',#9574,1.);
#2695=VECTOR('',#9577,1.);
#2696=VECTOR('',#9578,1.);
#2697=VECTOR('',#9579,1.);
#2698=VECTOR('',#9582,1.);
#2699=VECTOR('',#9583,1.);
#2700=VECTOR('',#9584,1.);
#2701=VECTOR('',#9585,1.);
#2702=VECTOR('',#9588,1.);
#2703=VECTOR('',#9589,1.);
#2704=VECTOR('',#9590,1.);
#2705=VECTOR('',#9593,1.);
#2706=VECTOR('',#9594,1.);
#2707=VECTOR('',#9595,1.);
#2708=VECTOR('',#9596,1.);
#2709=VECTOR('',#9599,1.);
#2710=VECTOR('',#9600,1.);
#2711=VECTOR('',#9601,1.);
#2712=VECTOR('',#9604,1.);
#2713=VECTOR('',#9605,1.);
#2714=VECTOR('',#9606,1.);
#2715=VECTOR('',#9607,1.);
#2716=VECTOR('',#9610,1.);
#2717=VECTOR('',#9611,1.);
#2718=VECTOR('',#9612,1.);
#2719=VECTOR('',#9615,1.);
#2720=VECTOR('',#9616,1.);
#2721=VECTOR('',#9617,1.);
#2722=VECTOR('',#9618,1.);
#2723=VECTOR('',#9621,1.);
#2724=VECTOR('',#9622,1.);
#2725=VECTOR('',#9623,1.);
#2726=VECTOR('',#9626,1.);
#2727=VECTOR('',#9627,1.);
#2728=VECTOR('',#9628,1.);
#2729=VECTOR('',#9629,1.);
#2730=VECTOR('',#9632,1.);
#2731=VECTOR('',#9633,1.);
#2732=VECTOR('',#9634,1.);
#2733=VECTOR('',#9637,1.);
#2734=VECTOR('',#9638,1.);
#2735=VECTOR('',#9639,1.);
#2736=VECTOR('',#9640,1.);
#2737=VECTOR('',#9643,1.);
#2738=VECTOR('',#9644,1.);
#2739=VECTOR('',#9645,1.);
#2740=VECTOR('',#9648,1.);
#2741=VECTOR('',#9649,1.);
#2742=VECTOR('',#9650,1.);
#2743=VECTOR('',#9651,1.);
#2744=VECTOR('',#9654,1.);
#2745=VECTOR('',#9655,1.);
#2746=VECTOR('',#9656,1.);
#2747=VECTOR('',#9659,1.);
#2748=VECTOR('',#9660,1.);
#2749=VECTOR('',#9661,1.);
#2750=VECTOR('',#9662,1.);
#2751=VECTOR('',#9665,1.);
#2752=VECTOR('',#9666,1.);
#2753=VECTOR('',#9667,1.);
#2754=VECTOR('',#9670,1.);
#2755=VECTOR('',#9671,1.);
#2756=VECTOR('',#9672,1.);
#2757=VECTOR('',#9673,1.);
#2758=VECTOR('',#9676,1.);
#2759=VECTOR('',#9677,1.);
#2760=VECTOR('',#9678,1.);
#2761=VECTOR('',#9681,1.);
#2762=VECTOR('',#9682,1.);
#2763=VECTOR('',#9683,1.);
#2764=VECTOR('',#9684,1.);
#2765=VECTOR('',#9687,1.);
#2766=VECTOR('',#9688,1.);
#2767=VECTOR('',#9689,1.);
#2768=VECTOR('',#9692,1.);
#2769=VECTOR('',#9693,1.);
#2770=VECTOR('',#9694,1.);
#2771=VECTOR('',#9695,1.);
#2772=VECTOR('',#9698,1.);
#2773=VECTOR('',#9699,1.);
#2774=VECTOR('',#9700,1.);
#2775=VECTOR('',#9703,1.);
#2776=VECTOR('',#9704,1.);
#2777=VECTOR('',#9705,1.);
#2778=VECTOR('',#9706,1.);
#2779=VECTOR('',#9709,1.);
#2780=VECTOR('',#9710,1.);
#2781=VECTOR('',#9711,1.);
#2782=VECTOR('',#9714,1.);
#2783=VECTOR('',#9715,1.);
#2784=VECTOR('',#9716,1.);
#2785=VECTOR('',#9717,1.);
#2786=VECTOR('',#9720,1.);
#2787=VECTOR('',#9721,1.);
#2788=VECTOR('',#9722,1.);
#2789=VECTOR('',#9725,1.);
#2790=VECTOR('',#9726,1.);
#2791=VECTOR('',#9727,1.);
#2792=VECTOR('',#9728,1.);
#2793=VECTOR('',#9731,1.);
#2794=VECTOR('',#9732,1.);
#2795=VECTOR('',#9733,1.);
#2796=VECTOR('',#9736,1.);
#2797=VECTOR('',#9737,1.);
#2798=VECTOR('',#9738,1.);
#2799=VECTOR('',#9739,1.);
#2800=VECTOR('',#9742,1.);
#2801=VECTOR('',#9743,1.);
#2802=VECTOR('',#9744,1.);
#2803=VECTOR('',#9747,1.);
#2804=VECTOR('',#9748,1.);
#2805=VECTOR('',#9749,1.);
#2806=VECTOR('',#9750,1.);
#2807=VECTOR('',#9753,1.);
#2808=VECTOR('',#9754,1.);
#2809=VECTOR('',#9755,1.);
#2810=VECTOR('',#9758,1.);
#2811=VECTOR('',#9759,1.);
#2812=VECTOR('',#9760,1.);
#2813=VECTOR('',#9761,1.);
#2814=VECTOR('',#9764,1.);
#2815=VECTOR('',#9765,1.);
#2816=VECTOR('',#9766,1.);
#2817=VECTOR('',#9769,1.);
#2818=VECTOR('',#9770,1.);
#2819=VECTOR('',#9771,1.);
#2820=VECTOR('',#9772,1.);
#2821=VECTOR('',#9775,1.);
#2822=VECTOR('',#9776,1.);
#2823=VECTOR('',#9777,1.);
#2824=VECTOR('',#9780,1.);
#2825=VECTOR('',#9781,1.);
#2826=VECTOR('',#9782,1.);
#2827=VECTOR('',#9783,1.);
#2828=VECTOR('',#9786,1.);
#2829=VECTOR('',#9787,1.);
#2830=VECTOR('',#9788,1.);
#2831=VECTOR('',#9791,1.);
#2832=VECTOR('',#9792,1.);
#2833=VECTOR('',#9793,1.);
#2834=VECTOR('',#9794,1.);
#2835=VECTOR('',#9797,1.);
#2836=VECTOR('',#9798,1.);
#2837=VECTOR('',#9799,1.);
#2838=VECTOR('',#9802,1.);
#2839=VECTOR('',#9803,1.);
#2840=VECTOR('',#9804,1.);
#2841=VECTOR('',#9805,1.);
#2842=VECTOR('',#9808,1.);
#2843=VECTOR('',#9809,1.);
#2844=VECTOR('',#9810,1.);
#2845=VECTOR('',#9813,1.);
#2846=VECTOR('',#9814,1.);
#2847=VECTOR('',#9815,1.);
#2848=VECTOR('',#9816,1.);
#2849=VECTOR('',#9819,1.);
#2850=VECTOR('',#9820,1.);
#2851=VECTOR('',#9821,1.);
#2852=VECTOR('',#9824,1.);
#2853=VECTOR('',#9825,1.);
#2854=VECTOR('',#9826,1.);
#2855=VECTOR('',#9827,1.);
#2856=VECTOR('',#9830,1.);
#2857=VECTOR('',#9831,1.);
#2858=VECTOR('',#9832,1.);
#2859=VECTOR('',#9835,1.);
#2860=VECTOR('',#9836,1.);
#2861=VECTOR('',#9837,1.);
#2862=VECTOR('',#9838,1.);
#2863=VECTOR('',#9841,1.);
#2864=VECTOR('',#9842,1.);
#2865=VECTOR('',#9843,1.);
#2866=VECTOR('',#9846,1.);
#2867=VECTOR('',#9847,1.);
#2868=VECTOR('',#9848,1.);
#2869=VECTOR('',#9849,1.);
#2870=VECTOR('',#9852,1.);
#2871=VECTOR('',#9853,1.);
#2872=VECTOR('',#9854,1.);
#2873=VECTOR('',#9857,1.);
#2874=VECTOR('',#9858,1.);
#2875=VECTOR('',#9859,1.);
#2876=VECTOR('',#9860,1.);
#2877=VECTOR('',#9863,1.);
#2878=VECTOR('',#9864,1.);
#2879=VECTOR('',#9865,1.);
#2880=VECTOR('',#9868,1.);
#2881=VECTOR('',#9869,1.);
#2882=VECTOR('',#9870,1.);
#2883=VECTOR('',#9871,1.);
#2884=VECTOR('',#9874,1.);
#2885=VECTOR('',#9875,1.);
#2886=VECTOR('',#9876,1.);
#2887=VECTOR('',#9879,1.);
#2888=VECTOR('',#9880,1.);
#2889=VECTOR('',#9881,1.);
#2890=VECTOR('',#9882,1.);
#2891=VECTOR('',#9885,1.);
#2892=VECTOR('',#9886,1.);
#2893=VECTOR('',#9887,1.);
#2894=VECTOR('',#9890,1.);
#2895=VECTOR('',#9891,1.);
#2896=VECTOR('',#9892,1.);
#2897=VECTOR('',#9893,1.);
#2898=VECTOR('',#9896,1.);
#2899=VECTOR('',#9897,1.);
#2900=VECTOR('',#9898,1.);
#2901=VECTOR('',#9901,1.);
#2902=VECTOR('',#9902,1.);
#2903=VECTOR('',#9903,1.);
#2904=VECTOR('',#9904,1.);
#2905=VECTOR('',#9907,1.);
#2906=VECTOR('',#9908,1.);
#2907=VECTOR('',#9909,1.);
#2908=VECTOR('',#9912,1.);
#2909=VECTOR('',#9913,1.);
#2910=VECTOR('',#9914,1.);
#2911=VECTOR('',#9915,1.);
#2912=VECTOR('',#9918,1.);
#2913=VECTOR('',#9919,1.);
#2914=VECTOR('',#9920,1.);
#2915=VECTOR('',#9923,1.);
#2916=VECTOR('',#9924,1.);
#2917=VECTOR('',#9925,1.);
#2918=VECTOR('',#9926,1.);
#2919=VECTOR('',#9929,1.);
#2920=VECTOR('',#9930,1.);
#2921=VECTOR('',#9931,1.);
#2922=VECTOR('',#9934,1.);
#2923=VECTOR('',#9935,1.);
#2924=VECTOR('',#9936,1.);
#2925=VECTOR('',#9937,1.);
#2926=VECTOR('',#9940,1.);
#2927=VECTOR('',#9941,1.);
#2928=VECTOR('',#9942,1.);
#2929=VECTOR('',#9945,1.);
#2930=VECTOR('',#9946,1.);
#2931=VECTOR('',#9947,1.);
#2932=VECTOR('',#9948,1.);
#2933=VECTOR('',#9949,1.);
#2934=VECTOR('',#9952,1.);
#2935=VECTOR('',#9953,1.);
#2936=VECTOR('',#9956,1.);
#2937=VECTOR('',#9957,1.);
#2938=VECTOR('',#9960,1.);
#2939=VECTOR('',#9961,1.);
#2940=VECTOR('',#9964,1.);
#2941=VECTOR('',#9965,1.);
#2942=VECTOR('',#9968,1.);
#2943=VECTOR('',#9969,1.);
#2944=VECTOR('',#9972,1.);
#2945=VECTOR('',#9973,1.);
#2946=VECTOR('',#9976,1.);
#2947=VECTOR('',#9977,1.);
#2948=VECTOR('',#9980,1.);
#2949=VECTOR('',#9981,1.);
#2950=VECTOR('',#9984,1.);
#2951=VECTOR('',#9985,1.);
#2952=VECTOR('',#9988,1.);
#2953=VECTOR('',#9989,1.);
#2954=VECTOR('',#9992,1.);
#2955=VECTOR('',#9993,1.);
#2956=VECTOR('',#9996,1.);
#2957=VECTOR('',#9997,1.);
#2958=VECTOR('',#10000,1.);
#2959=VECTOR('',#10001,1.);
#2960=VECTOR('',#10004,1.);
#2961=VECTOR('',#10005,1.);
#2962=VECTOR('',#10008,1.);
#2963=VECTOR('',#10009,1.);
#2964=VECTOR('',#10012,1.);
#2965=VECTOR('',#10013,1.);
#2966=VECTOR('',#10016,1.);
#2967=VECTOR('',#10017,1.);
#2968=VECTOR('',#10020,1.);
#2969=VECTOR('',#10021,1.);
#2970=VECTOR('',#10024,1.);
#2971=VECTOR('',#10025,1.);
#2972=VECTOR('',#10028,1.);
#2973=VECTOR('',#10029,1.);
#2974=VECTOR('',#10032,1.);
#2975=VECTOR('',#10033,1.);
#2976=VECTOR('',#10036,1.);
#2977=VECTOR('',#10037,1.);
#2978=VECTOR('',#10040,1.);
#2979=VECTOR('',#10041,1.);
#2980=VECTOR('',#10044,1.);
#2981=VECTOR('',#10045,1.);
#2982=VECTOR('',#10048,1.);
#2983=VECTOR('',#10049,1.);
#2984=VECTOR('',#10052,1.);
#2985=VECTOR('',#10053,1.);
#2986=VECTOR('',#10056,1.);
#2987=VECTOR('',#10057,1.);
#2988=VECTOR('',#10060,1.);
#2989=VECTOR('',#10061,1.);
#2990=VECTOR('',#10064,1.);
#2991=VECTOR('',#10065,1.);
#2992=VECTOR('',#10066,1.);
#2993=VECTOR('',#10069,1.);
#2994=VECTOR('',#10070,1.);
#2995=VECTOR('',#10073,1.);
#2996=VECTOR('',#10074,1.);
#2997=VECTOR('',#10077,1.);
#2998=VECTOR('',#10078,1.);
#2999=VECTOR('',#10081,1.);
#3000=VECTOR('',#10082,1.);
#3001=VECTOR('',#10085,1.);
#3002=VECTOR('',#10086,1.);
#3003=VECTOR('',#10089,1.);
#3004=VECTOR('',#10090,1.);
#3005=VECTOR('',#10093,1.);
#3006=VECTOR('',#10094,1.);
#3007=VECTOR('',#10097,1.);
#3008=VECTOR('',#10098,1.);
#3009=VECTOR('',#10101,1.);
#3010=VECTOR('',#10102,1.);
#3011=VECTOR('',#10105,1.);
#3012=VECTOR('',#10106,1.);
#3013=VECTOR('',#10107,1.);
#3014=VECTOR('',#10108,1.);
#3015=VECTOR('',#10111,1.);
#3016=VECTOR('',#10112,1.);
#3017=VECTOR('',#10115,1.);
#3018=VECTOR('',#10116,1.);
#3019=VECTOR('',#10117,1.);
#3020=VECTOR('',#10118,1.);
#3021=VECTOR('',#10121,1.);
#3022=VECTOR('',#10122,1.);
#3023=VECTOR('',#10125,1.);
#3024=VECTOR('',#10126,1.);
#3025=VECTOR('',#10129,1.);
#3026=VECTOR('',#10130,1.);
#3027=VECTOR('',#10135,1.);
#3028=VECTOR('',#10136,1.);
#3029=VECTOR('',#10137,1.);
#3030=VECTOR('',#10138,1.);
#3031=VECTOR('',#10139,1.);
#3032=VECTOR('',#10140,1.);
#3033=VECTOR('',#10147,1.);
#3034=VECTOR('',#10150,1.);
#3035=VECTOR('',#10151,1.);
#3036=VECTOR('',#10152,1.);
#3037=VECTOR('',#10155,1.);
#3038=VECTOR('',#10156,1.);
#3039=VECTOR('',#10159,1.);
#3040=VECTOR('',#10160,1.);
#3041=VECTOR('',#10163,1.);
#3042=VECTOR('',#10164,1.);
#3043=VECTOR('',#10167,1.);
#3044=VECTOR('',#10168,1.);
#3045=VECTOR('',#10171,1.);
#3046=VECTOR('',#10184,0.3);
#3047=VECTOR('',#10199,0.4);
#3048=VECTOR('',#10208,0.6);
#3049=VECTOR('',#10215,0.4);
#3050=VECTOR('',#10222,1.);
#3051=VECTOR('',#10223,1.);
#3052=VECTOR('',#10224,1.);
#3053=VECTOR('',#10225,1.);
#3054=VECTOR('',#10228,1.);
#3055=VECTOR('',#10229,1.);
#3056=VECTOR('',#10230,1.);
#3057=VECTOR('',#10231,1.);
#3058=VECTOR('',#10270,1.);
#3059=VECTOR('',#10271,1.);
#3060=VECTOR('',#10282,0.15);
#3061=VECTOR('',#10287,0.15);
#3062=VECTOR('',#10294,0.15);
#3063=VECTOR('',#10301,0.15);
#3064=VECTOR('',#10306,0.3);
#3065=VECTOR('',#10317,0.3);
#3066=VECTOR('',#10326,0.17);
#3067=VECTOR('',#10331,0.17);
#3068=VECTOR('',#10336,1.);
#3069=VECTOR('',#10337,1.);
#3070=VECTOR('',#10338,1.);
#3071=VECTOR('',#10339,1.);
#3072=VECTOR('',#10342,1.);
#3073=VECTOR('',#10343,1.);
#3074=VECTOR('',#10344,1.);
#3075=VECTOR('',#10345,1.);
#3076=VECTOR('',#10348,1.);
#3077=VECTOR('',#10349,1.);
#3078=VECTOR('',#10350,1.);
#3079=VECTOR('',#10351,1.);
#3080=VECTOR('',#10354,1.);
#3081=VECTOR('',#10355,1.);
#3082=VECTOR('',#10356,1.);
#3083=VECTOR('',#10357,1.);
#3084=VECTOR('',#10360,1.);
#3085=VECTOR('',#10361,1.);
#3086=VECTOR('',#10362,1.);
#3087=VECTOR('',#10363,1.);
#3088=VECTOR('',#10366,1.);
#3089=VECTOR('',#10367,1.);
#3090=VECTOR('',#10368,1.);
#3091=VECTOR('',#10369,1.);
#3092=VECTOR('',#10372,1.);
#3093=VECTOR('',#10373,1.);
#3094=VECTOR('',#10374,1.);
#3095=VECTOR('',#10375,1.);
#3096=VECTOR('',#10386,1.);
#3097=VECTOR('',#10387,1.);
#3098=VECTOR('',#10390,1.);
#3099=VECTOR('',#10391,1.);
#3100=VECTOR('',#10394,1.);
#3101=VECTOR('',#10395,1.);
#3102=VECTOR('',#10398,1.);
#3103=VECTOR('',#10399,1.);
#3104=VECTOR('',#10400,1.);
#3105=VECTOR('',#10403,1.);
#3106=VECTOR('',#10404,1.);
#3107=VECTOR('',#10405,1.);
#3108=VECTOR('',#10408,1.);
#3109=VECTOR('',#10411,1.);
#3110=VECTOR('',#10412,1.);
#3111=VECTOR('',#10415,1.);
#3112=VECTOR('',#10416,1.);
#3113=VECTOR('',#10417,1.);
#3114=VECTOR('',#10420,1.);
#3115=VECTOR('',#10421,1.);
#3116=VECTOR('',#10422,1.);
#3117=VECTOR('',#10425,1.);
#3118=VECTOR('',#10426,1.);
#3119=VECTOR('',#10427,1.);
#3120=VECTOR('',#10430,1.);
#3121=VECTOR('',#10431,1.);
#3122=VECTOR('',#10432,1.);
#3123=VECTOR('',#10433,1.);
#3124=VECTOR('',#10434,1.);
#3125=VECTOR('',#10435,1.);
#3126=VECTOR('',#10436,1.);
#3127=VECTOR('',#10437,1.);
#3128=VECTOR('',#10438,1.);
#3129=VECTOR('',#10439,1.);
#3130=VECTOR('',#10440,1.);
#3131=VECTOR('',#10443,0.4);
#3132=VECTOR('',#10448,0.4);
#3133=VECTOR('',#10451,1.);
#3134=VECTOR('',#10456,1.);
#3135=VECTOR('',#10459,1.);
#3136=VECTOR('',#10464,1.);
#3137=VECTOR('',#10469,1.);
#3138=VECTOR('',#10474,1.);
#3139=VECTOR('',#10507,1.);
#3140=VECTOR('',#10536,1.);
#3141=VECTOR('',#10537,1.);
#3142=VECTOR('',#10548,1.);
#3143=VECTOR('',#10549,1.);
#3144=VECTOR('',#10576,1.);
#3145=VECTOR('',#10577,1.);
#3146=VECTOR('',#10586,1.);
#3147=VECTOR('',#10587,1.);
#3148=VECTOR('',#10588,1.);
#3149=VECTOR('',#10589,1.);
#3150=VECTOR('',#10592,1.);
#3151=VECTOR('',#10593,1.);
#3152=VECTOR('',#10594,1.);
#3153=VECTOR('',#10597,1.);
#3154=VECTOR('',#10598,1.);
#3155=VECTOR('',#10599,1.);
#3156=VECTOR('',#10602,1.);
#3157=VECTOR('',#10603,1.);
#3158=VECTOR('',#10604,1.);
#3159=VECTOR('',#10607,1.);
#3160=VECTOR('',#10608,1.);
#3161=VECTOR('',#10609,1.);
#3162=VECTOR('',#10612,1.);
#3163=VECTOR('',#10613,1.);
#3164=VECTOR('',#10620,1.);
#3165=VECTOR('',#10621,1.);
#3166=VECTOR('',#10622,1.);
#3167=VECTOR('',#10623,1.);
#3168=VECTOR('',#10626,1.);
#3169=VECTOR('',#10627,1.);
#3170=VECTOR('',#10628,1.);
#3171=VECTOR('',#10631,1.);
#3172=VECTOR('',#10632,1.);
#3173=VECTOR('',#10633,1.);
#3174=VECTOR('',#10636,1.);
#3175=VECTOR('',#10637,1.);
#3176=VECTOR('',#10638,1.);
#3177=VECTOR('',#10641,1.);
#3178=VECTOR('',#10642,1.);
#3179=VECTOR('',#10643,1.);
#3180=VECTOR('',#10646,1.);
#3181=VECTOR('',#10647,1.);
#3182=VECTOR('',#10656,0.15);
#3183=VECTOR('',#10661,0.15);
#3184=VECTOR('',#10668,0.15);
#3185=VECTOR('',#10675,0.15);
#3186=VECTOR('',#10678,0.17);
#3187=VECTOR('',#10683,0.17);
#3188=VECTOR('',#10688,1.);
#3189=VECTOR('',#10689,1.);
#3190=VECTOR('',#10690,1.);
#3191=VECTOR('',#10691,1.);
#3192=VECTOR('',#10694,1.);
#3193=VECTOR('',#10695,1.);
#3194=VECTOR('',#10696,1.);
#3195=VECTOR('',#10697,1.);
#3196=VECTOR('',#10700,1.);
#3197=VECTOR('',#10701,1.);
#3198=VECTOR('',#10702,1.);
#3199=VECTOR('',#10703,1.);
#3200=VECTOR('',#10706,1.);
#3201=VECTOR('',#10707,1.);
#3202=VECTOR('',#10708,1.);
#3203=VECTOR('',#10709,1.);
#3204=VECTOR('',#10712,1.);
#3205=VECTOR('',#10713,1.);
#3206=VECTOR('',#10714,1.);
#3207=VECTOR('',#10715,1.);
#3208=VECTOR('',#10718,1.);
#3209=VECTOR('',#10719,1.);
#3210=VECTOR('',#10720,1.);
#3211=VECTOR('',#10721,1.);
#3212=VECTOR('',#10724,1.);
#3213=VECTOR('',#10725,1.);
#3214=VECTOR('',#10726,1.);
#3215=VECTOR('',#10727,1.);
#3216=VECTOR('',#10738,1.);
#3217=VECTOR('',#10739,1.);
#3218=VECTOR('',#10742,1.);
#3219=VECTOR('',#10743,1.);
#3220=VECTOR('',#10746,1.);
#3221=VECTOR('',#10747,1.);
#3222=VECTOR('',#10750,1.);
#3223=VECTOR('',#10751,1.);
#3224=VECTOR('',#10752,1.);
#3225=VECTOR('',#10755,1.);
#3226=VECTOR('',#10756,1.);
#3227=VECTOR('',#10757,1.);
#3228=VECTOR('',#10760,1.);
#3229=VECTOR('',#10763,1.);
#3230=VECTOR('',#10764,1.);
#3231=VECTOR('',#10767,1.);
#3232=VECTOR('',#10768,1.);
#3233=VECTOR('',#10769,1.);
#3234=VECTOR('',#10772,1.);
#3235=VECTOR('',#10773,1.);
#3236=VECTOR('',#10774,1.);
#3237=VECTOR('',#10777,1.);
#3238=VECTOR('',#10778,1.);
#3239=VECTOR('',#10779,1.);
#3240=VECTOR('',#10782,1.);
#3241=VECTOR('',#10783,1.);
#3242=VECTOR('',#10784,1.);
#3243=VECTOR('',#10785,1.);
#3244=VECTOR('',#10786,1.);
#3245=VECTOR('',#10787,1.);
#3246=VECTOR('',#10788,1.);
#3247=VECTOR('',#10789,1.);
#3248=VECTOR('',#10790,1.);
#3249=VECTOR('',#10791,1.);
#3250=VECTOR('',#10792,1.);
#3251=VECTOR('',#10795,0.4);
#3252=VECTOR('',#10800,0.4);
#3253=VECTOR('',#10803,1.);
#3254=VECTOR('',#10808,1.);
#3255=VECTOR('',#10811,1.);
#3256=VECTOR('',#10816,1.);
#3257=VECTOR('',#10821,1.);
#3258=VECTOR('',#10826,1.);
#3259=VECTOR('',#10859,1.);
#3260=VECTOR('',#10888,1.);
#3261=VECTOR('',#10889,1.);
#3262=VECTOR('',#10900,1.);
#3263=VECTOR('',#10901,1.);
#3264=VECTOR('',#10912,0.15);
#3265=VECTOR('',#10917,0.15);
#3266=VECTOR('',#10920,0.15);
#3267=VECTOR('',#10923,0.15);
#3268=VECTOR('',#10926,0.15);
#3269=VECTOR('',#10929,0.15);
#3270=VECTOR('',#10932,0.15);
#3271=VECTOR('',#10935,0.15);
#3272=VECTOR('',#10938,0.15);
#3273=VECTOR('',#10941,0.15);
#3274=VECTOR('',#10944,0.15);
#3275=VECTOR('',#10947,0.15);
#3276=VECTOR('',#10950,0.15);
#3277=VECTOR('',#10953,0.15);
#3278=VECTOR('',#10956,0.15);
#3279=VECTOR('',#10959,0.15);
#3280=VECTOR('',#10962,0.15);
#3281=VECTOR('',#10965,0.15);
#3282=VECTOR('',#10968,0.15);
#3283=VECTOR('',#10971,0.15);
#3284=VECTOR('',#10974,0.15);
#3285=VECTOR('',#10977,0.15);
#3286=VECTOR('',#10980,0.15);
#3287=VECTOR('',#10983,0.15);
#3288=VECTOR('',#10986,0.15);
#3289=VECTOR('',#10989,0.15);
#3290=VECTOR('',#10992,0.15);
#3291=VECTOR('',#10995,0.15);
#3292=VECTOR('',#10998,0.15);
#3293=VECTOR('',#11001,0.15);
#3294=VECTOR('',#11004,0.117775);
#3295=VECTOR('',#11009,0.117775);
#3296=VECTOR('',#11012,0.117775);
#3297=VECTOR('',#11015,0.117775);
#3298=VECTOR('',#11018,0.117775);
#3299=VECTOR('',#11021,0.117775);
#3300=VECTOR('',#11024,0.117775);
#3301=VECTOR('',#11027,0.117775);
#3302=VECTOR('',#11030,0.117775);
#3303=VECTOR('',#11033,0.117775);
#3304=VECTOR('',#11036,0.117775);
#3305=VECTOR('',#11039,0.117775);
#3306=VECTOR('',#11042,0.117775);
#3307=VECTOR('',#11045,0.117775);
#3308=VECTOR('',#11048,0.117775);
#3309=VECTOR('',#11051,0.117775);
#3310=VECTOR('',#11054,0.117775);
#3311=VECTOR('',#11057,0.117775);
#3312=VECTOR('',#11060,0.117775);
#3313=VECTOR('',#11063,0.117775);
#3314=VECTOR('',#11066,0.117775);
#3315=VECTOR('',#11069,0.117775);
#3316=VECTOR('',#11072,0.117775);
#3317=VECTOR('',#11075,0.117775);
#3318=VECTOR('',#11078,0.117775);
#3319=VECTOR('',#11081,0.117775);
#3320=VECTOR('',#11084,0.117775);
#3321=VECTOR('',#11087,0.117775);
#3322=VECTOR('',#11090,0.117775);
#3323=VECTOR('',#11093,0.117775);
#3324=VECTOR('',#11098,0.1);
#3325=VECTOR('',#11109,1.);
#3326=VECTOR('',#11110,1.);
#3327=VECTOR('',#11111,1.);
#3328=VECTOR('',#11112,1.);
#3329=VECTOR('',#11115,1.);
#3330=VECTOR('',#11116,1.);
#3331=VECTOR('',#11117,1.);
#3332=VECTOR('',#11120,1.);
#3333=VECTOR('',#11121,1.);
#3334=VECTOR('',#11122,1.);
#3335=VECTOR('',#11125,1.);
#3336=VECTOR('',#11126,1.);
#3337=VECTOR('',#11127,1.);
#3338=VECTOR('',#11130,1.);
#3339=VECTOR('',#11131,1.);
#3340=VECTOR('',#11132,1.);
#3341=VECTOR('',#11135,1.);
#3342=VECTOR('',#11136,1.);
#3343=VECTOR('',#11145,0.275);
#3344=VECTOR('',#11156,0.15);
#3345=VECTOR('',#11161,0.15);
#3346=VECTOR('',#11166,0.15);
#3347=VECTOR('',#11169,0.15);
#3348=VECTOR('',#11172,0.15);
#3349=VECTOR('',#11177,0.1543);
#3350=VECTOR('',#11182,0.1543);
#3351=VECTOR('',#11185,0.1543);
#3352=VECTOR('',#11188,0.1543);
#3353=VECTOR('',#11191,0.1543);
#3354=VECTOR('',#11198,1.);
#3355=VECTOR('',#11199,1.);
#3356=VECTOR('',#11200,1.);
#3357=VECTOR('',#11201,1.);
#3358=VECTOR('',#11202,1.);
#3359=VECTOR('',#11203,1.);
#3360=VECTOR('',#11208,1.);
#3361=VECTOR('',#11209,1.);
#3362=VECTOR('',#11210,1.);
#3363=VECTOR('',#11213,1.);
#3364=VECTOR('',#11214,1.);
#3365=VECTOR('',#11217,1.);
#3366=VECTOR('',#11218,1.);
#3367=VECTOR('',#11221,1.);
#3368=VECTOR('',#11222,1.);
#3369=VECTOR('',#11225,1.);
#3370=VECTOR('',#11226,1.);
#3371=VECTOR('',#11229,1.);
#3372=VECTOR('',#11238,0.35);
#3373=VECTOR('',#11245,0.35);
#3374=VECTOR('',#11258,0.25);
#3375=VECTOR('',#11271,0.25);
#3376=VECTOR('',#11284,0.25);
#3377=VECTOR('',#11297,0.25);
#3378=VECTOR('',#11302,0.15);
#3379=VECTOR('',#11307,0.15);
#3380=VECTOR('',#11312,0.15);
#3381=VECTOR('',#11317,0.15);
#3382=VECTOR('',#11328,1.);
#3383=VECTOR('',#11329,1.);
#3384=VECTOR('',#11340,1.);
#3385=VECTOR('',#11341,1.);
#3386=VECTOR('',#11346,1.);
#3387=VECTOR('',#11351,1.);
#3388=VECTOR('',#11376,0.41);
#3389=VECTOR('',#11383,0.6);
#3390=CIRCLE('',#8915,0.17);
#3391=CIRCLE('',#8916,0.17);
#3392=CIRCLE('',#8918,0.17);
#3393=CIRCLE('',#8919,0.17);
#3394=CIRCLE('',#8921,0.41);
#3395=CIRCLE('',#8922,0.41);
#3396=CIRCLE('',#9045,1.4);
#3397=CIRCLE('',#9046,1.4);
#3398=CIRCLE('',#9048,1.4);
#3399=CIRCLE('',#9056,1.4);
#3400=CIRCLE('',#9060,0.3);
#3401=CIRCLE('',#9061,0.3);
#3402=CIRCLE('',#9063,0.4);
#3403=CIRCLE('',#9065,0.4);
#3404=CIRCLE('',#9067,0.4);
#3405=CIRCLE('',#9069,0.6);
#3406=CIRCLE('',#9070,0.4);
#3407=CIRCLE('',#9072,0.6);
#3408=CIRCLE('',#9080,0.6);
#3409=CIRCLE('',#9081,0.3);
#3410=CIRCLE('',#9083,0.3);
#3411=CIRCLE('',#9085,0.6);
#3412=CIRCLE('',#9090,0.25);
#3413=CIRCLE('',#9092,0.25);
#3414=CIRCLE('',#9094,0.25);
#3415=CIRCLE('',#9096,0.25);
#3416=CIRCLE('',#9098,0.15);
#3417=CIRCLE('',#9099,0.15);
#3418=CIRCLE('',#9100,0.4);
#3419=CIRCLE('',#9102,0.15);
#3420=CIRCLE('',#9104,0.15);
#3421=CIRCLE('',#9105,0.15);
#3422=CIRCLE('',#9107,0.15);
#3423=CIRCLE('',#9108,0.15);
#3424=CIRCLE('',#9110,0.15);
#3425=CIRCLE('',#9112,0.3);
#3426=CIRCLE('',#9113,0.3);
#3427=CIRCLE('',#9115,0.17);
#3428=CIRCLE('',#9117,0.3);
#3429=CIRCLE('',#9118,0.3);
#3430=CIRCLE('',#9120,0.17);
#3431=CIRCLE('',#9122,0.17);
#3432=CIRCLE('',#9124,0.17);
#3433=CIRCLE('',#9133,0.4);
#3434=CIRCLE('',#9135,0.4);
#3435=CIRCLE('',#9149,0.4);
#3436=CIRCLE('',#9151,0.1);
#3437=CIRCLE('',#9158,0.0999999999999995);
#3438=CIRCLE('',#9160,0.1);
#3439=CIRCLE('',#9162,0.1);
#3440=CIRCLE('',#9163,0.1);
#3441=CIRCLE('',#9165,0.0999999999999999);
#3442=CIRCLE('',#9166,0.0999999999999998);
#3443=CIRCLE('',#9167,0.0999999999999998);
#3444=CIRCLE('',#9169,0.0999999999999994);
#3445=CIRCLE('',#9170,0.0999999999999993);
#3446=CIRCLE('',#9173,0.0999999999999999);
#3447=CIRCLE('',#9174,0.1);
#3448=CIRCLE('',#9178,0.3);
#3449=CIRCLE('',#9179,0.3);
#3450=CIRCLE('',#9180,0.3);
#3451=CIRCLE('',#9182,0.3);
#3452=CIRCLE('',#9183,0.3);
#3453=CIRCLE('',#9184,0.3);
#3454=CIRCLE('',#9186,0.3);
#3455=CIRCLE('',#9187,0.299999999999999);
#3456=CIRCLE('',#9188,0.3);
#3457=CIRCLE('',#9191,0.3);
#3458=CIRCLE('',#9192,0.3);
#3459=CIRCLE('',#9193,0.3);
#3460=CIRCLE('',#9200,0.25);
#3461=CIRCLE('',#9202,0.25);
#3462=CIRCLE('',#9204,0.25);
#3463=CIRCLE('',#9206,0.25);
#3464=CIRCLE('',#9208,0.15);
#3465=CIRCLE('',#9209,0.15);
#3466=CIRCLE('',#9210,0.4);
#3467=CIRCLE('',#9218,0.17);
#3468=CIRCLE('',#9226,0.17);
#3469=CIRCLE('',#9228,0.15);
#3470=CIRCLE('',#9230,0.15);
#3471=CIRCLE('',#9231,0.15);
#3472=CIRCLE('',#9233,0.15);
#3473=CIRCLE('',#9234,0.15);
#3474=CIRCLE('',#9236,0.15);
#3475=CIRCLE('',#9238,0.17);
#3476=CIRCLE('',#9240,0.17);
#3477=CIRCLE('',#9249,0.4);
#3478=CIRCLE('',#9251,0.4);
#3479=CIRCLE('',#9265,0.4);
#3480=CIRCLE('',#9267,0.1);
#3481=CIRCLE('',#9274,0.0999999999999995);
#3482=CIRCLE('',#9276,0.1);
#3483=CIRCLE('',#9278,0.1);
#3484=CIRCLE('',#9279,0.1);
#3485=CIRCLE('',#9281,0.0999999999999999);
#3486=CIRCLE('',#9282,0.0999999999999998);
#3487=CIRCLE('',#9283,0.0999999999999998);
#3488=CIRCLE('',#9285,0.0999999999999994);
#3489=CIRCLE('',#9286,0.0999999999999993);
#3490=CIRCLE('',#9289,0.0999999999999999);
#3491=CIRCLE('',#9290,0.1);
#3492=CIRCLE('',#9294,0.3);
#3493=CIRCLE('',#9295,0.3);
#3494=CIRCLE('',#9296,0.3);
#3495=CIRCLE('',#9298,0.3);
#3496=CIRCLE('',#9299,0.3);
#3497=CIRCLE('',#9300,0.3);
#3498=CIRCLE('',#9302,0.3);
#3499=CIRCLE('',#9303,0.299999999999999);
#3500=CIRCLE('',#9304,0.3);
#3501=CIRCLE('',#9307,0.3);
#3502=CIRCLE('',#9308,0.3);
#3503=CIRCLE('',#9309,0.3);
#3504=CIRCLE('',#9316,0.14635);
#3505=CIRCLE('',#9347,0.117775);
#3506=CIRCLE('',#9378,0.14635);
#3507=CIRCLE('',#9379,0.05);
#3508=CIRCLE('',#9381,0.117775);
#3509=CIRCLE('',#9391,0.275);
#3510=CIRCLE('',#9393,0.275);
#3511=CIRCLE('',#9398,0.12645);
#3512=CIRCLE('',#9400,0.12645);
#3513=CIRCLE('',#9404,0.12645);
#3514=CIRCLE('',#9406,0.1543);
#3515=CIRCLE('',#9411,0.1543);
#3516=CIRCLE('',#9424,0.35);
#3517=CIRCLE('',#9425,0.35);
#3518=CIRCLE('',#9427,0.35);
#3519=CIRCLE('',#9428,0.35);
#3520=CIRCLE('',#9430,0.25);
#3521=CIRCLE('',#9431,0.15);
#3522=CIRCLE('',#9433,0.25);
#3523=CIRCLE('',#9436,0.25);
#3524=CIRCLE('',#9437,0.15);
#3525=CIRCLE('',#9439,0.25);
#3526=CIRCLE('',#9442,0.25);
#3527=CIRCLE('',#9443,0.15);
#3528=CIRCLE('',#9445,0.25);
#3529=CIRCLE('',#9448,0.25);
#3530=CIRCLE('',#9449,0.15);
#3531=CIRCLE('',#9451,0.25);
#3532=CIRCLE('',#9454,0.15);
#3533=CIRCLE('',#9456,0.15);
#3534=CIRCLE('',#9458,0.15);
#3535=CIRCLE('',#9460,0.15);
#3536=CIRCLE('',#9461,0.0800000000000001);
#3537=CIRCLE('',#9462,0.0799999999999999);
#3538=CIRCLE('',#9464,0.0800000000000001);
#3539=CIRCLE('',#9465,0.0800000000000001);
#3540=CIRCLE('',#9466,0.0800000000000001);
#3541=CIRCLE('',#9467,0.0800000000000001);
#3542=CIRCLE('',#9469,0.0800000000000001);
#3543=CIRCLE('',#9470,0.0800000000000001);
#3544=CIRCLE('',#9485,0.41);
#3545=CIRCLE('',#9486,0.41);
#3546=CIRCLE('',#9488,0.6);
#3547=CIRCLE('',#9489,0.6);
#3548=VERTEX_POINT('',#11409);
#3549=VERTEX_POINT('',#11411);
#3550=VERTEX_POINT('',#11415);
#3551=VERTEX_POINT('',#11417);
#3552=VERTEX_POINT('',#11421);
#3553=VERTEX_POINT('',#11423);
#3554=VERTEX_POINT('',#11427);
#3555=VERTEX_POINT('',#11428);
#3556=VERTEX_POINT('',#11430);
#3557=VERTEX_POINT('',#11432);
#3558=VERTEX_POINT('',#11436);
#3559=VERTEX_POINT('',#11437);
#3560=VERTEX_POINT('',#11442);
#3561=VERTEX_POINT('',#11443);
#3562=VERTEX_POINT('',#11445);
#3563=VERTEX_POINT('',#11447);
#3564=VERTEX_POINT('',#11451);
#3565=VERTEX_POINT('',#11452);
#3566=VERTEX_POINT('',#11457);
#3567=VERTEX_POINT('',#11458);
#3568=VERTEX_POINT('',#11460);
#3569=VERTEX_POINT('',#11462);
#3570=VERTEX_POINT('',#11466);
#3571=VERTEX_POINT('',#11467);
#3572=VERTEX_POINT('',#11472);
#3573=VERTEX_POINT('',#11473);
#3574=VERTEX_POINT('',#11475);
#3575=VERTEX_POINT('',#11477);
#3576=VERTEX_POINT('',#11481);
#3577=VERTEX_POINT('',#11482);
#3578=VERTEX_POINT('',#11487);
#3579=VERTEX_POINT('',#11488);
#3580=VERTEX_POINT('',#11490);
#3581=VERTEX_POINT('',#11492);
#3582=VERTEX_POINT('',#11496);
#3583=VERTEX_POINT('',#11497);
#3584=VERTEX_POINT('',#11502);
#3585=VERTEX_POINT('',#11503);
#3586=VERTEX_POINT('',#11505);
#3587=VERTEX_POINT('',#11507);
#3588=VERTEX_POINT('',#11511);
#3589=VERTEX_POINT('',#11512);
#3590=VERTEX_POINT('',#11517);
#3591=VERTEX_POINT('',#11518);
#3592=VERTEX_POINT('',#11520);
#3593=VERTEX_POINT('',#11522);
#3594=VERTEX_POINT('',#11526);
#3595=VERTEX_POINT('',#11527);
#3596=VERTEX_POINT('',#11532);
#3597=VERTEX_POINT('',#11533);
#3598=VERTEX_POINT('',#11535);
#3599=VERTEX_POINT('',#11537);
#3600=VERTEX_POINT('',#11541);
#3601=VERTEX_POINT('',#11542);
#3602=VERTEX_POINT('',#11547);
#3603=VERTEX_POINT('',#11548);
#3604=VERTEX_POINT('',#11550);
#3605=VERTEX_POINT('',#11552);
#3606=VERTEX_POINT('',#11556);
#3607=VERTEX_POINT('',#11557);
#3608=VERTEX_POINT('',#11562);
#3609=VERTEX_POINT('',#11563);
#3610=VERTEX_POINT('',#11565);
#3611=VERTEX_POINT('',#11567);
#3612=VERTEX_POINT('',#11571);
#3613=VERTEX_POINT('',#11572);
#3614=VERTEX_POINT('',#11577);
#3615=VERTEX_POINT('',#11578);
#3616=VERTEX_POINT('',#11580);
#3617=VERTEX_POINT('',#11582);
#3618=VERTEX_POINT('',#11586);
#3619=VERTEX_POINT('',#11587);
#3620=VERTEX_POINT('',#11592);
#3621=VERTEX_POINT('',#11593);
#3622=VERTEX_POINT('',#11595);
#3623=VERTEX_POINT('',#11597);
#3624=VERTEX_POINT('',#11601);
#3625=VERTEX_POINT('',#11602);
#3626=VERTEX_POINT('',#11607);
#3627=VERTEX_POINT('',#11608);
#3628=VERTEX_POINT('',#11610);
#3629=VERTEX_POINT('',#11612);
#3630=VERTEX_POINT('',#11616);
#3631=VERTEX_POINT('',#11617);
#3632=VERTEX_POINT('',#11622);
#3633=VERTEX_POINT('',#11623);
#3634=VERTEX_POINT('',#11625);
#3635=VERTEX_POINT('',#11627);
#3636=VERTEX_POINT('',#11631);
#3637=VERTEX_POINT('',#11632);
#3638=VERTEX_POINT('',#11637);
#3639=VERTEX_POINT('',#11638);
#3640=VERTEX_POINT('',#11640);
#3641=VERTEX_POINT('',#11642);
#3642=VERTEX_POINT('',#11646);
#3643=VERTEX_POINT('',#11647);
#3644=VERTEX_POINT('',#11652);
#3645=VERTEX_POINT('',#11653);
#3646=VERTEX_POINT('',#11655);
#3647=VERTEX_POINT('',#11657);
#3648=VERTEX_POINT('',#11661);
#3649=VERTEX_POINT('',#11662);
#3650=VERTEX_POINT('',#11667);
#3651=VERTEX_POINT('',#11668);
#3652=VERTEX_POINT('',#11670);
#3653=VERTEX_POINT('',#11672);
#3654=VERTEX_POINT('',#11676);
#3655=VERTEX_POINT('',#11677);
#3656=VERTEX_POINT('',#11682);
#3657=VERTEX_POINT('',#11683);
#3658=VERTEX_POINT('',#11685);
#3659=VERTEX_POINT('',#11687);
#3660=VERTEX_POINT('',#11691);
#3661=VERTEX_POINT('',#11692);
#3662=VERTEX_POINT('',#11697);
#3663=VERTEX_POINT('',#11698);
#3664=VERTEX_POINT('',#11700);
#3665=VERTEX_POINT('',#11702);
#3666=VERTEX_POINT('',#11706);
#3667=VERTEX_POINT('',#11707);
#3668=VERTEX_POINT('',#11712);
#3669=VERTEX_POINT('',#11713);
#3670=VERTEX_POINT('',#11715);
#3671=VERTEX_POINT('',#11717);
#3672=VERTEX_POINT('',#11721);
#3673=VERTEX_POINT('',#11722);
#3674=VERTEX_POINT('',#11727);
#3675=VERTEX_POINT('',#11728);
#3676=VERTEX_POINT('',#11730);
#3677=VERTEX_POINT('',#11732);
#3678=VERTEX_POINT('',#11736);
#3679=VERTEX_POINT('',#11737);
#3680=VERTEX_POINT('',#11742);
#3681=VERTEX_POINT('',#11743);
#3682=VERTEX_POINT('',#11745);
#3683=VERTEX_POINT('',#11747);
#3684=VERTEX_POINT('',#11751);
#3685=VERTEX_POINT('',#11752);
#3686=VERTEX_POINT('',#11757);
#3687=VERTEX_POINT('',#11758);
#3688=VERTEX_POINT('',#11760);
#3689=VERTEX_POINT('',#11762);
#3690=VERTEX_POINT('',#11766);
#3691=VERTEX_POINT('',#11767);
#3692=VERTEX_POINT('',#11772);
#3693=VERTEX_POINT('',#11773);
#3694=VERTEX_POINT('',#11775);
#3695=VERTEX_POINT('',#11777);
#3696=VERTEX_POINT('',#11781);
#3697=VERTEX_POINT('',#11782);
#3698=VERTEX_POINT('',#11787);
#3699=VERTEX_POINT('',#11788);
#3700=VERTEX_POINT('',#11790);
#3701=VERTEX_POINT('',#11792);
#3702=VERTEX_POINT('',#11796);
#3703=VERTEX_POINT('',#11797);
#3704=VERTEX_POINT('',#11802);
#3705=VERTEX_POINT('',#11803);
#3706=VERTEX_POINT('',#11805);
#3707=VERTEX_POINT('',#11807);
#3708=VERTEX_POINT('',#11811);
#3709=VERTEX_POINT('',#11812);
#3710=VERTEX_POINT('',#11817);
#3711=VERTEX_POINT('',#11818);
#3712=VERTEX_POINT('',#11820);
#3713=VERTEX_POINT('',#11822);
#3714=VERTEX_POINT('',#11826);
#3715=VERTEX_POINT('',#11827);
#3716=VERTEX_POINT('',#11832);
#3717=VERTEX_POINT('',#11833);
#3718=VERTEX_POINT('',#11835);
#3719=VERTEX_POINT('',#11837);
#3720=VERTEX_POINT('',#11841);
#3721=VERTEX_POINT('',#11842);
#3722=VERTEX_POINT('',#11847);
#3723=VERTEX_POINT('',#11848);
#3724=VERTEX_POINT('',#11850);
#3725=VERTEX_POINT('',#11852);
#3726=VERTEX_POINT('',#11856);
#3727=VERTEX_POINT('',#11857);
#3728=VERTEX_POINT('',#11862);
#3729=VERTEX_POINT('',#11863);
#3730=VERTEX_POINT('',#11865);
#3731=VERTEX_POINT('',#11867);
#3732=VERTEX_POINT('',#11871);
#3733=VERTEX_POINT('',#11872);
#3734=VERTEX_POINT('',#11877);
#3735=VERTEX_POINT('',#11878);
#3736=VERTEX_POINT('',#11880);
#3737=VERTEX_POINT('',#11882);
#3738=VERTEX_POINT('',#11886);
#3739=VERTEX_POINT('',#11887);
#3740=VERTEX_POINT('',#11892);
#3741=VERTEX_POINT('',#11893);
#3742=VERTEX_POINT('',#11895);
#3743=VERTEX_POINT('',#11897);
#3744=VERTEX_POINT('',#11901);
#3745=VERTEX_POINT('',#11902);
#3746=VERTEX_POINT('',#11907);
#3747=VERTEX_POINT('',#11908);
#3748=VERTEX_POINT('',#11910);
#3749=VERTEX_POINT('',#11912);
#3750=VERTEX_POINT('',#11916);
#3751=VERTEX_POINT('',#11917);
#3752=VERTEX_POINT('',#11922);
#3753=VERTEX_POINT('',#11923);
#3754=VERTEX_POINT('',#11925);
#3755=VERTEX_POINT('',#11927);
#3756=VERTEX_POINT('',#11931);
#3757=VERTEX_POINT('',#11932);
#3758=VERTEX_POINT('',#11937);
#3759=VERTEX_POINT('',#11938);
#3760=VERTEX_POINT('',#11940);
#3761=VERTEX_POINT('',#11942);
#3762=VERTEX_POINT('',#11946);
#3763=VERTEX_POINT('',#11947);
#3764=VERTEX_POINT('',#11952);
#3765=VERTEX_POINT('',#11953);
#3766=VERTEX_POINT('',#11955);
#3767=VERTEX_POINT('',#11957);
#3768=VERTEX_POINT('',#11961);
#3769=VERTEX_POINT('',#11962);
#3770=VERTEX_POINT('',#11967);
#3771=VERTEX_POINT('',#11968);
#3772=VERTEX_POINT('',#11970);
#3773=VERTEX_POINT('',#11972);
#3774=VERTEX_POINT('',#11976);
#3775=VERTEX_POINT('',#11977);
#3776=VERTEX_POINT('',#11982);
#3777=VERTEX_POINT('',#11983);
#3778=VERTEX_POINT('',#11985);
#3779=VERTEX_POINT('',#11987);
#3780=VERTEX_POINT('',#11991);
#3781=VERTEX_POINT('',#11992);
#3782=VERTEX_POINT('',#11997);
#3783=VERTEX_POINT('',#11999);
#3784=VERTEX_POINT('',#12001);
#3785=VERTEX_POINT('',#12003);
#3786=VERTEX_POINT('',#12091);
#3787=VERTEX_POINT('',#12093);
#3788=VERTEX_POINT('',#12124);
#3789=VERTEX_POINT('',#12126);
#3790=VERTEX_POINT('',#12128);
#3791=VERTEX_POINT('',#12132);
#3792=VERTEX_POINT('',#12136);
#3793=VERTEX_POINT('',#12137);
#3794=VERTEX_POINT('',#12139);
#3795=VERTEX_POINT('',#12141);
#3796=VERTEX_POINT('',#12145);
#3797=VERTEX_POINT('',#12149);
#3798=VERTEX_POINT('',#12156);
#3799=VERTEX_POINT('',#12158);
#3800=VERTEX_POINT('',#12160);
#3801=VERTEX_POINT('',#12162);
#3802=VERTEX_POINT('',#12164);
#3803=VERTEX_POINT('',#12166);
#3804=VERTEX_POINT('',#12168);
#3805=VERTEX_POINT('',#12172);
#3806=VERTEX_POINT('',#12176);
#3807=VERTEX_POINT('',#12178);
#3808=VERTEX_POINT('',#12182);
#3809=VERTEX_POINT('',#12186);
#3810=VERTEX_POINT('',#12190);
#3811=VERTEX_POINT('',#12194);
#3812=VERTEX_POINT('',#12204);
#3813=VERTEX_POINT('',#12206);
#3814=VERTEX_POINT('',#12210);
#3815=VERTEX_POINT('',#12213);
#3816=VERTEX_POINT('',#12216);
#3817=VERTEX_POINT('',#12220);
#3818=VERTEX_POINT('',#12222);
#3819=VERTEX_POINT('',#12225);
#3820=VERTEX_POINT('',#12234);
#3821=VERTEX_POINT('',#12235);
#3822=VERTEX_POINT('',#12237);
#3823=VERTEX_POINT('',#12239);
#3824=VERTEX_POINT('',#12243);
#3825=VERTEX_POINT('',#12244);
#3826=VERTEX_POINT('',#12246);
#3827=VERTEX_POINT('',#12248);
#3828=VERTEX_POINT('',#12262);
#3829=VERTEX_POINT('',#12263);
#3830=VERTEX_POINT('',#12290);
#3831=VERTEX_POINT('',#12291);
#3832=VERTEX_POINT('',#12314);
#3833=VERTEX_POINT('',#12315);
#3834=VERTEX_POINT('',#12338);
#3835=VERTEX_POINT('',#12339);
#3836=VERTEX_POINT('',#12385);
#3837=VERTEX_POINT('',#12390);
#3838=VERTEX_POINT('',#12419);
#3839=VERTEX_POINT('',#12424);
#3840=VERTEX_POINT('',#12477);
#3841=VERTEX_POINT('',#12482);
#3842=VERTEX_POINT('',#12511);
#3843=VERTEX_POINT('',#12516);
#3844=VERTEX_POINT('',#12550);
#3845=VERTEX_POINT('',#12556);
#3846=VERTEX_POINT('',#12562);
#3847=VERTEX_POINT('',#12564);
#3848=VERTEX_POINT('',#12566);
#3849=VERTEX_POINT('',#12569);
#3850=VERTEX_POINT('',#12573);
#3851=VERTEX_POINT('',#12575);
#3852=VERTEX_POINT('',#12579);
#3853=VERTEX_POINT('',#12581);
#3854=VERTEX_POINT('',#12585);
#3855=VERTEX_POINT('',#12589);
#3856=VERTEX_POINT('',#12591);
#3857=VERTEX_POINT('',#12595);
#3858=VERTEX_POINT('',#12598);
#3859=VERTEX_POINT('',#12600);
#3860=VERTEX_POINT('',#12604);
#3861=VERTEX_POINT('',#12607);
#3862=VERTEX_POINT('',#12611);
#3863=VERTEX_POINT('',#12615);
#3864=VERTEX_POINT('',#12616);
#3865=VERTEX_POINT('',#12618);
#3866=VERTEX_POINT('',#12620);
#3867=VERTEX_POINT('',#12624);
#3868=VERTEX_POINT('',#12625);
#3869=VERTEX_POINT('',#12627);
#3870=VERTEX_POINT('',#12629);
#3871=VERTEX_POINT('',#12633);
#3872=VERTEX_POINT('',#12634);
#3873=VERTEX_POINT('',#12636);
#3874=VERTEX_POINT('',#12638);
#3875=VERTEX_POINT('',#12642);
#3876=VERTEX_POINT('',#12643);
#3877=VERTEX_POINT('',#12645);
#3878=VERTEX_POINT('',#12647);
#3879=VERTEX_POINT('',#12651);
#3880=VERTEX_POINT('',#12652);
#3881=VERTEX_POINT('',#12654);
#3882=VERTEX_POINT('',#12656);
#3883=VERTEX_POINT('',#12660);
#3884=VERTEX_POINT('',#12661);
#3885=VERTEX_POINT('',#12663);
#3886=VERTEX_POINT('',#12665);
#3887=VERTEX_POINT('',#12669);
#3888=VERTEX_POINT('',#12670);
#3889=VERTEX_POINT('',#12672);
#3890=VERTEX_POINT('',#12674);
#3891=VERTEX_POINT('',#12678);
#3892=VERTEX_POINT('',#12681);
#3893=VERTEX_POINT('',#12693);
#3894=VERTEX_POINT('',#12695);
#3895=VERTEX_POINT('',#12699);
#3896=VERTEX_POINT('',#12701);
#3897=VERTEX_POINT('',#12705);
#3898=VERTEX_POINT('',#12706);
#3899=VERTEX_POINT('',#12708);
#3900=VERTEX_POINT('',#12750);
#3901=VERTEX_POINT('',#12758);
#3902=VERTEX_POINT('',#12787);
#3903=VERTEX_POINT('',#12796);
#3904=VERTEX_POINT('',#12798);
#3905=VERTEX_POINT('',#12805);
#3906=VERTEX_POINT('',#12834);
#3907=VERTEX_POINT('',#12836);
#3908=VERTEX_POINT('',#12865);
#3909=VERTEX_POINT('',#12874);
#3910=VERTEX_POINT('',#12882);
#3911=VERTEX_POINT('',#12884);
#3912=VERTEX_POINT('',#12913);
#3913=VERTEX_POINT('',#12922);
#3914=VERTEX_POINT('',#12924);
#3915=VERTEX_POINT('',#12929);
#3916=VERTEX_POINT('',#12931);
#3917=VERTEX_POINT('',#12946);
#3918=VERTEX_POINT('',#12955);
#3919=VERTEX_POINT('',#12961);
#3920=VERTEX_POINT('',#12963);
#3921=VERTEX_POINT('',#12996);
#3922=VERTEX_POINT('',#12998);
#3923=VERTEX_POINT('',#13030);
#3924=VERTEX_POINT('',#13035);
#3925=VERTEX_POINT('',#13067);
#3926=VERTEX_POINT('',#13069);
#3927=VERTEX_POINT('',#13101);
#3928=VERTEX_POINT('',#13106);
#3929=VERTEX_POINT('',#13139);
#3930=VERTEX_POINT('',#13165);
#3931=VERTEX_POINT('',#13171);
#3932=VERTEX_POINT('',#13177);
#3933=VERTEX_POINT('',#13186);
#3934=VERTEX_POINT('',#13187);
#3935=VERTEX_POINT('',#13192);
#3936=VERTEX_POINT('',#13221);
#3937=VERTEX_POINT('',#13223);
#3938=VERTEX_POINT('',#13252);
#3939=VERTEX_POINT('',#13261);
#3940=VERTEX_POINT('',#13265);
#3941=VERTEX_POINT('',#13272);
#3942=VERTEX_POINT('',#13279);
#3943=VERTEX_POINT('',#13308);
#3944=VERTEX_POINT('',#13374);
#3945=VERTEX_POINT('',#13423);
#3946=VERTEX_POINT('',#13430);
#3947=VERTEX_POINT('',#13468);
#3948=VERTEX_POINT('',#13478);
#3949=VERTEX_POINT('',#13485);
#3950=VERTEX_POINT('',#13514);
#3951=VERTEX_POINT('',#13516);
#3952=VERTEX_POINT('',#13641);
#3953=VERTEX_POINT('',#13648);
#3954=VERTEX_POINT('',#13750);
#3955=VERTEX_POINT('',#13757);
#3956=VERTEX_POINT('',#13786);
#3957=VERTEX_POINT('',#13788);
#3958=VERTEX_POINT('',#13839);
#3959=VERTEX_POINT('',#13868);
#3960=VERTEX_POINT('',#13875);
#3961=VERTEX_POINT('',#13897);
#3962=VERTEX_POINT('',#13932);
#3963=VERTEX_POINT('',#13960);
#3964=VERTEX_POINT('',#14055);
#3965=VERTEX_POINT('',#14056);
#3966=VERTEX_POINT('',#14058);
#3967=VERTEX_POINT('',#14062);
#3968=VERTEX_POINT('',#14063);
#3969=VERTEX_POINT('',#14065);
#3970=VERTEX_POINT('',#14069);
#3971=VERTEX_POINT('',#14070);
#3972=VERTEX_POINT('',#14072);
#3973=VERTEX_POINT('',#14107);
#3974=VERTEX_POINT('',#14108);
#3975=VERTEX_POINT('',#14110);
#3976=VERTEX_POINT('',#14307);
#3977=VERTEX_POINT('',#14308);
#3978=VERTEX_POINT('',#14335);
#3979=VERTEX_POINT('',#14336);
#3980=VERTEX_POINT('',#14359);
#3981=VERTEX_POINT('',#14360);
#3982=VERTEX_POINT('',#14383);
#3983=VERTEX_POINT('',#14384);
#3984=VERTEX_POINT('',#14430);
#3985=VERTEX_POINT('',#14435);
#3986=VERTEX_POINT('',#14464);
#3987=VERTEX_POINT('',#14469);
#3988=VERTEX_POINT('',#14522);
#3989=VERTEX_POINT('',#14527);
#3990=VERTEX_POINT('',#14556);
#3991=VERTEX_POINT('',#14561);
#3992=VERTEX_POINT('',#14595);
#3993=VERTEX_POINT('',#14601);
#3994=VERTEX_POINT('',#14607);
#3995=VERTEX_POINT('',#14609);
#3996=VERTEX_POINT('',#14611);
#3997=VERTEX_POINT('',#14614);
#3998=VERTEX_POINT('',#14615);
#3999=VERTEX_POINT('',#14617);
#4000=VERTEX_POINT('',#14619);
#4001=VERTEX_POINT('',#14623);
#4002=VERTEX_POINT('',#14625);
#4003=VERTEX_POINT('',#14629);
#4004=VERTEX_POINT('',#14631);
#4005=VERTEX_POINT('',#14635);
#4006=VERTEX_POINT('',#14637);
#4007=VERTEX_POINT('',#14641);
#4008=VERTEX_POINT('',#14643);
#4009=VERTEX_POINT('',#14650);
#4010=VERTEX_POINT('',#14653);
#4011=VERTEX_POINT('',#14654);
#4012=VERTEX_POINT('',#14656);
#4013=VERTEX_POINT('',#14658);
#4014=VERTEX_POINT('',#14662);
#4015=VERTEX_POINT('',#14664);
#4016=VERTEX_POINT('',#14668);
#4017=VERTEX_POINT('',#14670);
#4018=VERTEX_POINT('',#14674);
#4019=VERTEX_POINT('',#14676);
#4020=VERTEX_POINT('',#14680);
#4021=VERTEX_POINT('',#14682);
#4022=VERTEX_POINT('',#14689);
#4023=VERTEX_POINT('',#14692);
#4024=VERTEX_POINT('',#14696);
#4025=VERTEX_POINT('',#14698);
#4026=VERTEX_POINT('',#14702);
#4027=VERTEX_POINT('',#14704);
#4028=VERTEX_POINT('',#14708);
#4029=VERTEX_POINT('',#14712);
#4030=VERTEX_POINT('',#14716);
#4031=VERTEX_POINT('',#14720);
#4032=VERTEX_POINT('',#14721);
#4033=VERTEX_POINT('',#14723);
#4034=VERTEX_POINT('',#14725);
#4035=VERTEX_POINT('',#14729);
#4036=VERTEX_POINT('',#14730);
#4037=VERTEX_POINT('',#14732);
#4038=VERTEX_POINT('',#14734);
#4039=VERTEX_POINT('',#14738);
#4040=VERTEX_POINT('',#14739);
#4041=VERTEX_POINT('',#14741);
#4042=VERTEX_POINT('',#14743);
#4043=VERTEX_POINT('',#14747);
#4044=VERTEX_POINT('',#14748);
#4045=VERTEX_POINT('',#14750);
#4046=VERTEX_POINT('',#14752);
#4047=VERTEX_POINT('',#14756);
#4048=VERTEX_POINT('',#14757);
#4049=VERTEX_POINT('',#14759);
#4050=VERTEX_POINT('',#14761);
#4051=VERTEX_POINT('',#14765);
#4052=VERTEX_POINT('',#14766);
#4053=VERTEX_POINT('',#14768);
#4054=VERTEX_POINT('',#14770);
#4055=VERTEX_POINT('',#14774);
#4056=VERTEX_POINT('',#14775);
#4057=VERTEX_POINT('',#14777);
#4058=VERTEX_POINT('',#14779);
#4059=VERTEX_POINT('',#14783);
#4060=VERTEX_POINT('',#14786);
#4061=VERTEX_POINT('',#14798);
#4062=VERTEX_POINT('',#14800);
#4063=VERTEX_POINT('',#14804);
#4064=VERTEX_POINT('',#14806);
#4065=VERTEX_POINT('',#14810);
#4066=VERTEX_POINT('',#14811);
#4067=VERTEX_POINT('',#14813);
#4068=VERTEX_POINT('',#14855);
#4069=VERTEX_POINT('',#14863);
#4070=VERTEX_POINT('',#14892);
#4071=VERTEX_POINT('',#14901);
#4072=VERTEX_POINT('',#14903);
#4073=VERTEX_POINT('',#14910);
#4074=VERTEX_POINT('',#14939);
#4075=VERTEX_POINT('',#14941);
#4076=VERTEX_POINT('',#14970);
#4077=VERTEX_POINT('',#14979);
#4078=VERTEX_POINT('',#14987);
#4079=VERTEX_POINT('',#14989);
#4080=VERTEX_POINT('',#15018);
#4081=VERTEX_POINT('',#15027);
#4082=VERTEX_POINT('',#15029);
#4083=VERTEX_POINT('',#15034);
#4084=VERTEX_POINT('',#15036);
#4085=VERTEX_POINT('',#15051);
#4086=VERTEX_POINT('',#15060);
#4087=VERTEX_POINT('',#15066);
#4088=VERTEX_POINT('',#15068);
#4089=VERTEX_POINT('',#15101);
#4090=VERTEX_POINT('',#15103);
#4091=VERTEX_POINT('',#15135);
#4092=VERTEX_POINT('',#15140);
#4093=VERTEX_POINT('',#15172);
#4094=VERTEX_POINT('',#15174);
#4095=VERTEX_POINT('',#15206);
#4096=VERTEX_POINT('',#15211);
#4097=VERTEX_POINT('',#15244);
#4098=VERTEX_POINT('',#15270);
#4099=VERTEX_POINT('',#15276);
#4100=VERTEX_POINT('',#15282);
#4101=VERTEX_POINT('',#15291);
#4102=VERTEX_POINT('',#15292);
#4103=VERTEX_POINT('',#15297);
#4104=VERTEX_POINT('',#15326);
#4105=VERTEX_POINT('',#15328);
#4106=VERTEX_POINT('',#15357);
#4107=VERTEX_POINT('',#15366);
#4108=VERTEX_POINT('',#15370);
#4109=VERTEX_POINT('',#15377);
#4110=VERTEX_POINT('',#15384);
#4111=VERTEX_POINT('',#15413);
#4112=VERTEX_POINT('',#15479);
#4113=VERTEX_POINT('',#15528);
#4114=VERTEX_POINT('',#15535);
#4115=VERTEX_POINT('',#15573);
#4116=VERTEX_POINT('',#15583);
#4117=VERTEX_POINT('',#15590);
#4118=VERTEX_POINT('',#15619);
#4119=VERTEX_POINT('',#15621);
#4120=VERTEX_POINT('',#15746);
#4121=VERTEX_POINT('',#15753);
#4122=VERTEX_POINT('',#15855);
#4123=VERTEX_POINT('',#15862);
#4124=VERTEX_POINT('',#15891);
#4125=VERTEX_POINT('',#15893);
#4126=VERTEX_POINT('',#15944);
#4127=VERTEX_POINT('',#15973);
#4128=VERTEX_POINT('',#15980);
#4129=VERTEX_POINT('',#16002);
#4130=VERTEX_POINT('',#16037);
#4131=VERTEX_POINT('',#16065);
#4132=VERTEX_POINT('',#16160);
#4133=VERTEX_POINT('',#16161);
#4134=VERTEX_POINT('',#16163);
#4135=VERTEX_POINT('',#16167);
#4136=VERTEX_POINT('',#16168);
#4137=VERTEX_POINT('',#16170);
#4138=VERTEX_POINT('',#16174);
#4139=VERTEX_POINT('',#16175);
#4140=VERTEX_POINT('',#16177);
#4141=VERTEX_POINT('',#16212);
#4142=VERTEX_POINT('',#16213);
#4143=VERTEX_POINT('',#16215);
#4144=VERTEX_POINT('',#16412);
#4145=VERTEX_POINT('',#16413);
#4146=VERTEX_POINT('',#16415);
#4147=VERTEX_POINT('',#16426);
#4148=VERTEX_POINT('',#16436);
#4149=VERTEX_POINT('',#16437);
#4150=VERTEX_POINT('',#16484);
#4151=VERTEX_POINT('',#16485);
#4152=VERTEX_POINT('',#16532);
#4153=VERTEX_POINT('',#16533);
#4154=VERTEX_POINT('',#16583);
#4155=VERTEX_POINT('',#16584);
#4156=VERTEX_POINT('',#16631);
#4157=VERTEX_POINT('',#16632);
#4158=VERTEX_POINT('',#16679);
#4159=VERTEX_POINT('',#16680);
#4160=VERTEX_POINT('',#16727);
#4161=VERTEX_POINT('',#16728);
#4162=VERTEX_POINT('',#16781);
#4163=VERTEX_POINT('',#16782);
#4164=VERTEX_POINT('',#16829);
#4165=VERTEX_POINT('',#16830);
#4166=VERTEX_POINT('',#16877);
#4167=VERTEX_POINT('',#16878);
#4168=VERTEX_POINT('',#16931);
#4169=VERTEX_POINT('',#16932);
#4170=VERTEX_POINT('',#16979);
#4171=VERTEX_POINT('',#16980);
#4172=VERTEX_POINT('',#17027);
#4173=VERTEX_POINT('',#17028);
#4174=VERTEX_POINT('',#17075);
#4175=VERTEX_POINT('',#17076);
#4176=VERTEX_POINT('',#17129);
#4177=VERTEX_POINT('',#17130);
#4178=VERTEX_POINT('',#17177);
#4179=VERTEX_POINT('',#17178);
#4180=VERTEX_POINT('',#17225);
#4181=VERTEX_POINT('',#17226);
#4182=VERTEX_POINT('',#17279);
#4183=VERTEX_POINT('',#17280);
#4184=VERTEX_POINT('',#17327);
#4185=VERTEX_POINT('',#17328);
#4186=VERTEX_POINT('',#17375);
#4187=VERTEX_POINT('',#17376);
#4188=VERTEX_POINT('',#17429);
#4189=VERTEX_POINT('',#17430);
#4190=VERTEX_POINT('',#17477);
#4191=VERTEX_POINT('',#17478);
#4192=VERTEX_POINT('',#17525);
#4193=VERTEX_POINT('',#17526);
#4194=VERTEX_POINT('',#17573);
#4195=VERTEX_POINT('',#17574);
#4196=VERTEX_POINT('',#17627);
#4197=VERTEX_POINT('',#17628);
#4198=VERTEX_POINT('',#17675);
#4199=VERTEX_POINT('',#17676);
#4200=VERTEX_POINT('',#17723);
#4201=VERTEX_POINT('',#17724);
#4202=VERTEX_POINT('',#17777);
#4203=VERTEX_POINT('',#17778);
#4204=VERTEX_POINT('',#17825);
#4205=VERTEX_POINT('',#17826);
#4206=VERTEX_POINT('',#17873);
#4207=VERTEX_POINT('',#17874);
#4208=VERTEX_POINT('',#17876);
#4209=VERTEX_POINT('',#17887);
#4210=VERTEX_POINT('',#17899);
#4211=VERTEX_POINT('',#17900);
#4212=VERTEX_POINT('',#17923);
#4213=VERTEX_POINT('',#17924);
#4214=VERTEX_POINT('',#17947);
#4215=VERTEX_POINT('',#17948);
#4216=VERTEX_POINT('',#17972);
#4217=VERTEX_POINT('',#17973);
#4218=VERTEX_POINT('',#17997);
#4219=VERTEX_POINT('',#17998);
#4220=VERTEX_POINT('',#18021);
#4221=VERTEX_POINT('',#18022);
#4222=VERTEX_POINT('',#18046);
#4223=VERTEX_POINT('',#18047);
#4224=VERTEX_POINT('',#18071);
#4225=VERTEX_POINT('',#18072);
#4226=VERTEX_POINT('',#18095);
#4227=VERTEX_POINT('',#18096);
#4228=VERTEX_POINT('',#18119);
#4229=VERTEX_POINT('',#18120);
#4230=VERTEX_POINT('',#18144);
#4231=VERTEX_POINT('',#18145);
#4232=VERTEX_POINT('',#18169);
#4233=VERTEX_POINT('',#18170);
#4234=VERTEX_POINT('',#18193);
#4235=VERTEX_POINT('',#18194);
#4236=VERTEX_POINT('',#18218);
#4237=VERTEX_POINT('',#18219);
#4238=VERTEX_POINT('',#18243);
#4239=VERTEX_POINT('',#18244);
#4240=VERTEX_POINT('',#18267);
#4241=VERTEX_POINT('',#18268);
#4242=VERTEX_POINT('',#18292);
#4243=VERTEX_POINT('',#18293);
#4244=VERTEX_POINT('',#18317);
#4245=VERTEX_POINT('',#18318);
#4246=VERTEX_POINT('',#18341);
#4247=VERTEX_POINT('',#18342);
#4248=VERTEX_POINT('',#18365);
#4249=VERTEX_POINT('',#18366);
#4250=VERTEX_POINT('',#18390);
#4251=VERTEX_POINT('',#18391);
#4252=VERTEX_POINT('',#18415);
#4253=VERTEX_POINT('',#18416);
#4254=VERTEX_POINT('',#18439);
#4255=VERTEX_POINT('',#18440);
#4256=VERTEX_POINT('',#18464);
#4257=VERTEX_POINT('',#18465);
#4258=VERTEX_POINT('',#18489);
#4259=VERTEX_POINT('',#18490);
#4260=VERTEX_POINT('',#18513);
#4261=VERTEX_POINT('',#18514);
#4262=VERTEX_POINT('',#18538);
#4263=VERTEX_POINT('',#18539);
#4264=VERTEX_POINT('',#18562);
#4265=VERTEX_POINT('',#18563);
#4266=VERTEX_POINT('',#18587);
#4267=VERTEX_POINT('',#18588);
#4268=VERTEX_POINT('',#18611);
#4269=VERTEX_POINT('',#18733);
#4270=VERTEX_POINT('',#18771);
#4271=VERTEX_POINT('',#18789);
#4272=VERTEX_POINT('',#19576);
#4273=VERTEX_POINT('',#19654);
#4274=VERTEX_POINT('',#20533);
#4275=VERTEX_POINT('',#20534);
#4276=VERTEX_POINT('',#20536);
#4277=VERTEX_POINT('',#20538);
#4278=VERTEX_POINT('',#20542);
#4279=VERTEX_POINT('',#20544);
#4280=VERTEX_POINT('',#20548);
#4281=VERTEX_POINT('',#20550);
#4282=VERTEX_POINT('',#20554);
#4283=VERTEX_POINT('',#20556);
#4284=VERTEX_POINT('',#20560);
#4285=VERTEX_POINT('',#20562);
#4286=VERTEX_POINT('',#20570);
#4287=VERTEX_POINT('',#20573);
#4288=VERTEX_POINT('',#20580);
#4289=VERTEX_POINT('',#20581);
#4290=VERTEX_POINT('',#20583);
#4291=VERTEX_POINT('',#20593);
#4292=VERTEX_POINT('',#20594);
#4293=VERTEX_POINT('',#20596);
#4294=VERTEX_POINT('',#20640);
#4295=VERTEX_POINT('',#20641);
#4296=VERTEX_POINT('',#20694);
#4297=VERTEX_POINT('',#20695);
#4298=VERTEX_POINT('',#20742);
#4299=VERTEX_POINT('',#20743);
#4300=VERTEX_POINT('',#20745);
#4301=VERTEX_POINT('',#20759);
#4302=VERTEX_POINT('',#20781);
#4303=VERTEX_POINT('',#20782);
#4304=VERTEX_POINT('',#20784);
#4305=VERTEX_POINT('',#20792);
#4306=VERTEX_POINT('',#20802);
#4307=VERTEX_POINT('',#20803);
#4308=VERTEX_POINT('',#20827);
#4309=VERTEX_POINT('',#20828);
#4310=VERTEX_POINT('',#20852);
#4311=VERTEX_POINT('',#20853);
#4312=VERTEX_POINT('',#20877);
#4313=VERTEX_POINT('',#20878);
#4314=VERTEX_POINT('',#20880);
#4315=VERTEX_POINT('',#20886);
#4316=VERTEX_POINT('',#21450);
#4317=VERTEX_POINT('',#21451);
#4318=VERTEX_POINT('',#21453);
#4319=VERTEX_POINT('',#21455);
#4320=VERTEX_POINT('',#21457);
#4321=VERTEX_POINT('',#21459);
#4322=VERTEX_POINT('',#21464);
#4323=VERTEX_POINT('',#21465);
#4324=VERTEX_POINT('',#21470);
#4325=VERTEX_POINT('',#21474);
#4326=VERTEX_POINT('',#21478);
#4327=VERTEX_POINT('',#21482);
#4328=VERTEX_POINT('',#21490);
#4329=VERTEX_POINT('',#21492);
#4330=VERTEX_POINT('',#21496);
#4331=VERTEX_POINT('',#21498);
#4332=VERTEX_POINT('',#21502);
#4333=VERTEX_POINT('',#21504);
#4334=VERTEX_POINT('',#21507);
#4335=VERTEX_POINT('',#21512);
#4336=VERTEX_POINT('',#21514);
#4337=VERTEX_POINT('',#21517);
#4338=VERTEX_POINT('',#21522);
#4339=VERTEX_POINT('',#21524);
#4340=VERTEX_POINT('',#21527);
#4341=VERTEX_POINT('',#21532);
#4342=VERTEX_POINT('',#21534);
#4343=VERTEX_POINT('',#21537);
#4344=VERTEX_POINT('',#21542);
#4345=VERTEX_POINT('',#21546);
#4346=VERTEX_POINT('',#21550);
#4347=VERTEX_POINT('',#21554);
#4348=VERTEX_POINT('',#21582);
#4349=VERTEX_POINT('',#21583);
#4350=VERTEX_POINT('',#21585);
#4351=VERTEX_POINT('',#21591);
#4352=VERTEX_POINT('',#21599);
#4353=VERTEX_POINT('',#21600);
#4354=VERTEX_POINT('',#21629);
#4355=VERTEX_POINT('',#21630);
#4356=VERTEX_POINT('',#21667);
#4357=VERTEX_POINT('',#21668);
#4358=VERTEX_POINT('',#21705);
#4359=VERTEX_POINT('',#21706);
#4360=VERTEX_POINT('',#21719);
#4361=VERTEX_POINT('',#21720);
#4362=VERTEX_POINT('',#21749);
#4363=VERTEX_POINT('',#21750);
#4364=VERTEX_POINT('',#21798);
#4365=VERTEX_POINT('',#21803);
#4366=VERTEX_POINT('',#21829);
#4367=VERTEX_POINT('',#21878);
#4368=VERTEX_POINT('',#21907);
#4369=VERTEX_POINT('',#21942);
#4370=VERTEX_POINT('',#21968);
#4371=VERTEX_POINT('',#22021);
#4372=VERTEX_POINT('',#22085);
#4373=VERTEX_POINT('',#22087);
#4374=VERTEX_POINT('',#22091);
#4375=VERTEX_POINT('',#22093);
#4376=EDGE_CURVE('',#3548,#3548,#3390,.T.);
#4377=EDGE_CURVE('',#3548,#3549,#1930,.T.);
#4378=EDGE_CURVE('',#3549,#3549,#3391,.T.);
#4379=EDGE_CURVE('',#3550,#3550,#3392,.T.);
#4380=EDGE_CURVE('',#3550,#3551,#1931,.T.);
#4381=EDGE_CURVE('',#3551,#3551,#3393,.T.);
#4382=EDGE_CURVE('',#3552,#3552,#3394,.T.);
#4383=EDGE_CURVE('',#3552,#3553,#1932,.T.);
#4384=EDGE_CURVE('',#3553,#3553,#3395,.T.);
#4385=EDGE_CURVE('',#3554,#3555,#1933,.T.);
#4386=EDGE_CURVE('',#3556,#3554,#1934,.T.);
#4387=EDGE_CURVE('',#3556,#3557,#1935,.T.);
#4388=EDGE_CURVE('',#3555,#3557,#1936,.T.);
#4389=EDGE_CURVE('',#3558,#3559,#1937,.T.);
#4390=EDGE_CURVE('',#3557,#3558,#1938,.T.);
#4391=EDGE_CURVE('',#3559,#3556,#1939,.T.);
#4392=EDGE_CURVE('',#3560,#3561,#1940,.T.);
#4393=EDGE_CURVE('',#3562,#3560,#1941,.T.);
#4394=EDGE_CURVE('',#3562,#3563,#1942,.T.);
#4395=EDGE_CURVE('',#3561,#3563,#1943,.T.);
#4396=EDGE_CURVE('',#3564,#3565,#1944,.T.);
#4397=EDGE_CURVE('',#3563,#3564,#1945,.T.);
#4398=EDGE_CURVE('',#3565,#3562,#1946,.T.);
#4399=EDGE_CURVE('',#3566,#3567,#1947,.T.);
#4400=EDGE_CURVE('',#3568,#3566,#1948,.T.);
#4401=EDGE_CURVE('',#3568,#3569,#1949,.T.);
#4402=EDGE_CURVE('',#3567,#3569,#1950,.T.);
#4403=EDGE_CURVE('',#3570,#3571,#1951,.T.);
#4404=EDGE_CURVE('',#3569,#3570,#1952,.T.);
#4405=EDGE_CURVE('',#3571,#3568,#1953,.T.);
#4406=EDGE_CURVE('',#3572,#3573,#1954,.T.);
#4407=EDGE_CURVE('',#3574,#3572,#1955,.T.);
#4408=EDGE_CURVE('',#3574,#3575,#1956,.T.);
#4409=EDGE_CURVE('',#3573,#3575,#1957,.T.);
#4410=EDGE_CURVE('',#3576,#3577,#1958,.T.);
#4411=EDGE_CURVE('',#3575,#3576,#1959,.T.);
#4412=EDGE_CURVE('',#3577,#3574,#1960,.T.);
#4413=EDGE_CURVE('',#3578,#3579,#1961,.T.);
#4414=EDGE_CURVE('',#3580,#3578,#1962,.T.);
#4415=EDGE_CURVE('',#3580,#3581,#1963,.T.);
#4416=EDGE_CURVE('',#3579,#3581,#1964,.T.);
#4417=EDGE_CURVE('',#3582,#3583,#1965,.T.);
#4418=EDGE_CURVE('',#3581,#3582,#1966,.T.);
#4419=EDGE_CURVE('',#3583,#3580,#1967,.T.);
#4420=EDGE_CURVE('',#3584,#3585,#1968,.T.);
#4421=EDGE_CURVE('',#3586,#3584,#1969,.T.);
#4422=EDGE_CURVE('',#3586,#3587,#1970,.T.);
#4423=EDGE_CURVE('',#3585,#3587,#1971,.T.);
#4424=EDGE_CURVE('',#3588,#3589,#1972,.T.);
#4425=EDGE_CURVE('',#3587,#3588,#1973,.T.);
#4426=EDGE_CURVE('',#3589,#3586,#1974,.T.);
#4427=EDGE_CURVE('',#3590,#3591,#1975,.T.);
#4428=EDGE_CURVE('',#3592,#3590,#1976,.T.);
#4429=EDGE_CURVE('',#3592,#3593,#1977,.T.);
#4430=EDGE_CURVE('',#3591,#3593,#1978,.T.);
#4431=EDGE_CURVE('',#3594,#3595,#1979,.T.);
#4432=EDGE_CURVE('',#3593,#3594,#1980,.T.);
#4433=EDGE_CURVE('',#3595,#3592,#1981,.T.);
#4434=EDGE_CURVE('',#3596,#3597,#1982,.T.);
#4435=EDGE_CURVE('',#3598,#3596,#1983,.T.);
#4436=EDGE_CURVE('',#3598,#3599,#1984,.T.);
#4437=EDGE_CURVE('',#3597,#3599,#1985,.T.);
#4438=EDGE_CURVE('',#3600,#3601,#1986,.T.);
#4439=EDGE_CURVE('',#3599,#3600,#1987,.T.);
#4440=EDGE_CURVE('',#3601,#3598,#1988,.T.);
#4441=EDGE_CURVE('',#3602,#3603,#1989,.T.);
#4442=EDGE_CURVE('',#3604,#3602,#1990,.T.);
#4443=EDGE_CURVE('',#3604,#3605,#1991,.T.);
#4444=EDGE_CURVE('',#3603,#3605,#1992,.T.);
#4445=EDGE_CURVE('',#3606,#3607,#1993,.T.);
#4446=EDGE_CURVE('',#3605,#3606,#1994,.T.);
#4447=EDGE_CURVE('',#3607,#3604,#1995,.T.);
#4448=EDGE_CURVE('',#3608,#3609,#1996,.T.);
#4449=EDGE_CURVE('',#3610,#3608,#1997,.T.);
#4450=EDGE_CURVE('',#3610,#3611,#1998,.T.);
#4451=EDGE_CURVE('',#3609,#3611,#1999,.T.);
#4452=EDGE_CURVE('',#3612,#3613,#2000,.T.);
#4453=EDGE_CURVE('',#3611,#3612,#2001,.T.);
#4454=EDGE_CURVE('',#3613,#3610,#2002,.T.);
#4455=EDGE_CURVE('',#3614,#3615,#2003,.T.);
#4456=EDGE_CURVE('',#3616,#3614,#2004,.T.);
#4457=EDGE_CURVE('',#3616,#3617,#2005,.T.);
#4458=EDGE_CURVE('',#3615,#3617,#2006,.T.);
#4459=EDGE_CURVE('',#3618,#3619,#2007,.T.);
#4460=EDGE_CURVE('',#3617,#3618,#2008,.T.);
#4461=EDGE_CURVE('',#3619,#3616,#2009,.T.);
#4462=EDGE_CURVE('',#3620,#3621,#2010,.T.);
#4463=EDGE_CURVE('',#3622,#3620,#2011,.T.);
#4464=EDGE_CURVE('',#3622,#3623,#2012,.T.);
#4465=EDGE_CURVE('',#3621,#3623,#2013,.T.);
#4466=EDGE_CURVE('',#3624,#3625,#2014,.T.);
#4467=EDGE_CURVE('',#3623,#3624,#2015,.T.);
#4468=EDGE_CURVE('',#3625,#3622,#2016,.T.);
#4469=EDGE_CURVE('',#3626,#3627,#2017,.T.);
#4470=EDGE_CURVE('',#3628,#3626,#2018,.T.);
#4471=EDGE_CURVE('',#3628,#3629,#2019,.T.);
#4472=EDGE_CURVE('',#3627,#3629,#2020,.T.);
#4473=EDGE_CURVE('',#3630,#3631,#2021,.T.);
#4474=EDGE_CURVE('',#3629,#3630,#2022,.T.);
#4475=EDGE_CURVE('',#3631,#3628,#2023,.T.);
#4476=EDGE_CURVE('',#3632,#3633,#2024,.T.);
#4477=EDGE_CURVE('',#3634,#3632,#2025,.T.);
#4478=EDGE_CURVE('',#3634,#3635,#2026,.T.);
#4479=EDGE_CURVE('',#3633,#3635,#2027,.T.);
#4480=EDGE_CURVE('',#3636,#3637,#2028,.T.);
#4481=EDGE_CURVE('',#3635,#3636,#2029,.T.);
#4482=EDGE_CURVE('',#3637,#3634,#2030,.T.);
#4483=EDGE_CURVE('',#3638,#3639,#2031,.T.);
#4484=EDGE_CURVE('',#3640,#3638,#2032,.T.);
#4485=EDGE_CURVE('',#3640,#3641,#2033,.T.);
#4486=EDGE_CURVE('',#3639,#3641,#2034,.T.);
#4487=EDGE_CURVE('',#3642,#3643,#2035,.T.);
#4488=EDGE_CURVE('',#3641,#3642,#2036,.T.);
#4489=EDGE_CURVE('',#3643,#3640,#2037,.T.);
#4490=EDGE_CURVE('',#3644,#3645,#2038,.T.);
#4491=EDGE_CURVE('',#3646,#3644,#2039,.T.);
#4492=EDGE_CURVE('',#3646,#3647,#2040,.T.);
#4493=EDGE_CURVE('',#3645,#3647,#2041,.T.);
#4494=EDGE_CURVE('',#3648,#3649,#2042,.T.);
#4495=EDGE_CURVE('',#3647,#3648,#2043,.T.);
#4496=EDGE_CURVE('',#3649,#3646,#2044,.T.);
#4497=EDGE_CURVE('',#3650,#3651,#2045,.T.);
#4498=EDGE_CURVE('',#3652,#3650,#2046,.T.);
#4499=EDGE_CURVE('',#3652,#3653,#2047,.T.);
#4500=EDGE_CURVE('',#3651,#3653,#2048,.T.);
#4501=EDGE_CURVE('',#3654,#3655,#2049,.T.);
#4502=EDGE_CURVE('',#3653,#3654,#2050,.T.);
#4503=EDGE_CURVE('',#3655,#3652,#2051,.T.);
#4504=EDGE_CURVE('',#3656,#3657,#2052,.T.);
#4505=EDGE_CURVE('',#3658,#3656,#2053,.T.);
#4506=EDGE_CURVE('',#3658,#3659,#2054,.T.);
#4507=EDGE_CURVE('',#3657,#3659,#2055,.T.);
#4508=EDGE_CURVE('',#3660,#3661,#2056,.T.);
#4509=EDGE_CURVE('',#3659,#3660,#2057,.T.);
#4510=EDGE_CURVE('',#3661,#3658,#2058,.T.);
#4511=EDGE_CURVE('',#3662,#3663,#2059,.T.);
#4512=EDGE_CURVE('',#3664,#3662,#2060,.T.);
#4513=EDGE_CURVE('',#3664,#3665,#2061,.T.);
#4514=EDGE_CURVE('',#3663,#3665,#2062,.T.);
#4515=EDGE_CURVE('',#3666,#3667,#2063,.T.);
#4516=EDGE_CURVE('',#3665,#3666,#2064,.T.);
#4517=EDGE_CURVE('',#3667,#3664,#2065,.T.);
#4518=EDGE_CURVE('',#3668,#3669,#2066,.T.);
#4519=EDGE_CURVE('',#3670,#3668,#2067,.T.);
#4520=EDGE_CURVE('',#3670,#3671,#2068,.T.);
#4521=EDGE_CURVE('',#3669,#3671,#2069,.T.);
#4522=EDGE_CURVE('',#3672,#3673,#2070,.T.);
#4523=EDGE_CURVE('',#3671,#3672,#2071,.T.);
#4524=EDGE_CURVE('',#3673,#3670,#2072,.T.);
#4525=EDGE_CURVE('',#3674,#3675,#2073,.T.);
#4526=EDGE_CURVE('',#3676,#3674,#2074,.T.);
#4527=EDGE_CURVE('',#3676,#3677,#2075,.T.);
#4528=EDGE_CURVE('',#3675,#3677,#2076,.T.);
#4529=EDGE_CURVE('',#3678,#3679,#2077,.T.);
#4530=EDGE_CURVE('',#3677,#3678,#2078,.T.);
#4531=EDGE_CURVE('',#3679,#3676,#2079,.T.);
#4532=EDGE_CURVE('',#3680,#3681,#2080,.T.);
#4533=EDGE_CURVE('',#3682,#3680,#2081,.T.);
#4534=EDGE_CURVE('',#3682,#3683,#2082,.T.);
#4535=EDGE_CURVE('',#3681,#3683,#2083,.T.);
#4536=EDGE_CURVE('',#3684,#3685,#2084,.T.);
#4537=EDGE_CURVE('',#3683,#3684,#2085,.T.);
#4538=EDGE_CURVE('',#3685,#3682,#2086,.T.);
#4539=EDGE_CURVE('',#3686,#3687,#2087,.T.);
#4540=EDGE_CURVE('',#3688,#3686,#2088,.T.);
#4541=EDGE_CURVE('',#3688,#3689,#2089,.T.);
#4542=EDGE_CURVE('',#3687,#3689,#2090,.T.);
#4543=EDGE_CURVE('',#3690,#3691,#2091,.T.);
#4544=EDGE_CURVE('',#3689,#3690,#2092,.T.);
#4545=EDGE_CURVE('',#3691,#3688,#2093,.T.);
#4546=EDGE_CURVE('',#3692,#3693,#2094,.T.);
#4547=EDGE_CURVE('',#3694,#3692,#2095,.T.);
#4548=EDGE_CURVE('',#3694,#3695,#2096,.T.);
#4549=EDGE_CURVE('',#3693,#3695,#2097,.T.);
#4550=EDGE_CURVE('',#3696,#3697,#2098,.T.);
#4551=EDGE_CURVE('',#3695,#3696,#2099,.T.);
#4552=EDGE_CURVE('',#3697,#3694,#2100,.T.);
#4553=EDGE_CURVE('',#3698,#3699,#2101,.T.);
#4554=EDGE_CURVE('',#3700,#3698,#2102,.T.);
#4555=EDGE_CURVE('',#3700,#3701,#2103,.T.);
#4556=EDGE_CURVE('',#3699,#3701,#2104,.T.);
#4557=EDGE_CURVE('',#3702,#3703,#2105,.T.);
#4558=EDGE_CURVE('',#3701,#3702,#2106,.T.);
#4559=EDGE_CURVE('',#3703,#3700,#2107,.T.);
#4560=EDGE_CURVE('',#3704,#3705,#2108,.T.);
#4561=EDGE_CURVE('',#3706,#3704,#2109,.T.);
#4562=EDGE_CURVE('',#3706,#3707,#2110,.T.);
#4563=EDGE_CURVE('',#3705,#3707,#2111,.T.);
#4564=EDGE_CURVE('',#3708,#3709,#2112,.T.);
#4565=EDGE_CURVE('',#3707,#3708,#2113,.T.);
#4566=EDGE_CURVE('',#3709,#3706,#2114,.T.);
#4567=EDGE_CURVE('',#3710,#3711,#2115,.T.);
#4568=EDGE_CURVE('',#3712,#3710,#2116,.T.);
#4569=EDGE_CURVE('',#3712,#3713,#2117,.T.);
#4570=EDGE_CURVE('',#3711,#3713,#2118,.T.);
#4571=EDGE_CURVE('',#3714,#3715,#2119,.T.);
#4572=EDGE_CURVE('',#3713,#3714,#2120,.T.);
#4573=EDGE_CURVE('',#3715,#3712,#2121,.T.);
#4574=EDGE_CURVE('',#3716,#3717,#2122,.T.);
#4575=EDGE_CURVE('',#3718,#3716,#2123,.T.);
#4576=EDGE_CURVE('',#3718,#3719,#2124,.T.);
#4577=EDGE_CURVE('',#3717,#3719,#2125,.T.);
#4578=EDGE_CURVE('',#3720,#3721,#2126,.T.);
#4579=EDGE_CURVE('',#3719,#3720,#2127,.T.);
#4580=EDGE_CURVE('',#3721,#3718,#2128,.T.);
#4581=EDGE_CURVE('',#3722,#3723,#2129,.T.);
#4582=EDGE_CURVE('',#3724,#3722,#2130,.T.);
#4583=EDGE_CURVE('',#3724,#3725,#2131,.T.);
#4584=EDGE_CURVE('',#3723,#3725,#2132,.T.);
#4585=EDGE_CURVE('',#3726,#3727,#2133,.T.);
#4586=EDGE_CURVE('',#3725,#3726,#2134,.T.);
#4587=EDGE_CURVE('',#3727,#3724,#2135,.T.);
#4588=EDGE_CURVE('',#3728,#3729,#2136,.T.);
#4589=EDGE_CURVE('',#3730,#3728,#2137,.T.);
#4590=EDGE_CURVE('',#3730,#3731,#2138,.T.);
#4591=EDGE_CURVE('',#3729,#3731,#2139,.T.);
#4592=EDGE_CURVE('',#3732,#3733,#2140,.T.);
#4593=EDGE_CURVE('',#3731,#3732,#2141,.T.);
#4594=EDGE_CURVE('',#3733,#3730,#2142,.T.);
#4595=EDGE_CURVE('',#3734,#3735,#2143,.T.);
#4596=EDGE_CURVE('',#3736,#3734,#2144,.T.);
#4597=EDGE_CURVE('',#3736,#3737,#2145,.T.);
#4598=EDGE_CURVE('',#3735,#3737,#2146,.T.);
#4599=EDGE_CURVE('',#3738,#3739,#2147,.T.);
#4600=EDGE_CURVE('',#3737,#3738,#2148,.T.);
#4601=EDGE_CURVE('',#3739,#3736,#2149,.T.);
#4602=EDGE_CURVE('',#3740,#3741,#2150,.T.);
#4603=EDGE_CURVE('',#3742,#3740,#2151,.T.);
#4604=EDGE_CURVE('',#3742,#3743,#2152,.T.);
#4605=EDGE_CURVE('',#3741,#3743,#2153,.T.);
#4606=EDGE_CURVE('',#3744,#3745,#2154,.T.);
#4607=EDGE_CURVE('',#3743,#3744,#2155,.T.);
#4608=EDGE_CURVE('',#3745,#3742,#2156,.T.);
#4609=EDGE_CURVE('',#3746,#3747,#2157,.T.);
#4610=EDGE_CURVE('',#3748,#3746,#2158,.T.);
#4611=EDGE_CURVE('',#3748,#3749,#2159,.T.);
#4612=EDGE_CURVE('',#3747,#3749,#2160,.T.);
#4613=EDGE_CURVE('',#3750,#3751,#2161,.T.);
#4614=EDGE_CURVE('',#3749,#3750,#2162,.T.);
#4615=EDGE_CURVE('',#3751,#3748,#2163,.T.);
#4616=EDGE_CURVE('',#3752,#3753,#2164,.T.);
#4617=EDGE_CURVE('',#3754,#3752,#2165,.T.);
#4618=EDGE_CURVE('',#3754,#3755,#2166,.T.);
#4619=EDGE_CURVE('',#3753,#3755,#2167,.T.);
#4620=EDGE_CURVE('',#3756,#3757,#2168,.T.);
#4621=EDGE_CURVE('',#3755,#3756,#2169,.T.);
#4622=EDGE_CURVE('',#3757,#3754,#2170,.T.);
#4623=EDGE_CURVE('',#3758,#3759,#2171,.T.);
#4624=EDGE_CURVE('',#3760,#3758,#2172,.T.);
#4625=EDGE_CURVE('',#3760,#3761,#2173,.T.);
#4626=EDGE_CURVE('',#3759,#3761,#2174,.T.);
#4627=EDGE_CURVE('',#3762,#3763,#2175,.T.);
#4628=EDGE_CURVE('',#3761,#3762,#2176,.T.);
#4629=EDGE_CURVE('',#3763,#3760,#2177,.T.);
#4630=EDGE_CURVE('',#3764,#3765,#2178,.T.);
#4631=EDGE_CURVE('',#3766,#3764,#2179,.T.);
#4632=EDGE_CURVE('',#3766,#3767,#2180,.T.);
#4633=EDGE_CURVE('',#3765,#3767,#2181,.T.);
#4634=EDGE_CURVE('',#3768,#3769,#2182,.T.);
#4635=EDGE_CURVE('',#3767,#3768,#2183,.T.);
#4636=EDGE_CURVE('',#3769,#3766,#2184,.T.);
#4637=EDGE_CURVE('',#3770,#3771,#2185,.T.);
#4638=EDGE_CURVE('',#3772,#3770,#2186,.T.);
#4639=EDGE_CURVE('',#3772,#3773,#2187,.T.);
#4640=EDGE_CURVE('',#3771,#3773,#2188,.T.);
#4641=EDGE_CURVE('',#3774,#3775,#2189,.T.);
#4642=EDGE_CURVE('',#3773,#3774,#2190,.T.);
#4643=EDGE_CURVE('',#3775,#3772,#2191,.T.);
#4644=EDGE_CURVE('',#3776,#3777,#2192,.T.);
#4645=EDGE_CURVE('',#3778,#3776,#2193,.T.);
#4646=EDGE_CURVE('',#3778,#3779,#2194,.T.);
#4647=EDGE_CURVE('',#3777,#3779,#2195,.T.);
#4648=EDGE_CURVE('',#3780,#3781,#2196,.T.);
#4649=EDGE_CURVE('',#3779,#3780,#2197,.T.);
#4650=EDGE_CURVE('',#3781,#3778,#2198,.T.);
#4651=EDGE_CURVE('',#3782,#3777,#2199,.T.);
#4652=EDGE_CURVE('',#3782,#3783,#2200,.T.);
#4653=EDGE_CURVE('',#3784,#3783,#2201,.T.);
#4654=EDGE_CURVE('',#3785,#3784,#2202,.T.);
#4655=EDGE_CURVE('',#3776,#3785,#2203,.T.);
#4656=EDGE_CURVE('',#3780,#3555,#2204,.T.);
#4657=EDGE_CURVE('',#3554,#3781,#2205,.T.);
#4658=EDGE_CURVE('',#3774,#3561,#2206,.T.);
#4659=EDGE_CURVE('',#3560,#3775,#2207,.T.);
#4660=EDGE_CURVE('',#3768,#3567,#2208,.T.);
#4661=EDGE_CURVE('',#3566,#3769,#2209,.T.);
#4662=EDGE_CURVE('',#3762,#3573,#2210,.T.);
#4663=EDGE_CURVE('',#3572,#3763,#2211,.T.);
#4664=EDGE_CURVE('',#3756,#3579,#2212,.T.);
#4665=EDGE_CURVE('',#3578,#3757,#2213,.T.);
#4666=EDGE_CURVE('',#3750,#3585,#2214,.T.);
#4667=EDGE_CURVE('',#3584,#3751,#2215,.T.);
#4668=EDGE_CURVE('',#3744,#3591,#2216,.T.);
#4669=EDGE_CURVE('',#3590,#3745,#2217,.T.);
#4670=EDGE_CURVE('',#3738,#3597,#2218,.T.);
#4671=EDGE_CURVE('',#3596,#3739,#2219,.T.);
#4672=EDGE_CURVE('',#3732,#3603,#2220,.T.);
#4673=EDGE_CURVE('',#3602,#3733,#2221,.T.);
#4674=EDGE_CURVE('',#3726,#3717,#2222,.T.);
#4675=EDGE_CURVE('',#3716,#3727,#2223,.T.);
#4676=EDGE_CURVE('',#3720,#3615,#2224,.T.);
#4677=EDGE_CURVE('',#3614,#3721,#2225,.T.);
#4678=EDGE_CURVE('',#3714,#3621,#2226,.T.);
#4679=EDGE_CURVE('',#3620,#3715,#2227,.T.);
#4680=EDGE_CURVE('',#3708,#3627,#2228,.T.);
#4681=EDGE_CURVE('',#3626,#3709,#2229,.T.);
#4682=EDGE_CURVE('',#3702,#3633,#2230,.T.);
#4683=EDGE_CURVE('',#3632,#3703,#2231,.T.);
#4684=EDGE_CURVE('',#3696,#3639,#2232,.T.);
#4685=EDGE_CURVE('',#3638,#3697,#2233,.T.);
#4686=EDGE_CURVE('',#3690,#3645,#2234,.T.);
#4687=EDGE_CURVE('',#3644,#3691,#2235,.T.);
#4688=EDGE_CURVE('',#3684,#3651,#2236,.T.);
#4689=EDGE_CURVE('',#3650,#3685,#2237,.T.);
#4690=EDGE_CURVE('',#3678,#3657,#2238,.T.);
#4691=EDGE_CURVE('',#3656,#3679,#2239,.T.);
#4692=EDGE_CURVE('',#3672,#3663,#2240,.T.);
#4693=EDGE_CURVE('',#3662,#3673,#2241,.T.);
#4694=EDGE_CURVE('',#3666,#3609,#2242,.T.);
#4695=EDGE_CURVE('',#3608,#3667,#2243,.T.);
#4696=EDGE_CURVE('',#3668,#3661,#2244,.T.);
#4697=EDGE_CURVE('',#3660,#3669,#2245,.T.);
#4698=EDGE_CURVE('',#3674,#3655,#2246,.T.);
#4699=EDGE_CURVE('',#3654,#3675,#2247,.T.);
#4700=EDGE_CURVE('',#3680,#3649,#2248,.T.);
#4701=EDGE_CURVE('',#3648,#3681,#2249,.T.);
#4702=EDGE_CURVE('',#3686,#3643,#2250,.T.);
#4703=EDGE_CURVE('',#3642,#3687,#2251,.T.);
#4704=EDGE_CURVE('',#3692,#3637,#2252,.T.);
#4705=EDGE_CURVE('',#3636,#3693,#2253,.T.);
#4706=EDGE_CURVE('',#3698,#3631,#2254,.T.);
#4707=EDGE_CURVE('',#3630,#3699,#2255,.T.);
#4708=EDGE_CURVE('',#3704,#3625,#2256,.T.);
#4709=EDGE_CURVE('',#3624,#3705,#2257,.T.);
#4710=EDGE_CURVE('',#3710,#3619,#2258,.T.);
#4711=EDGE_CURVE('',#3618,#3711,#2259,.T.);
#4712=EDGE_CURVE('',#3786,#3613,#2260,.T.);
#4713=EDGE_CURVE('',#3787,#3786,#2261,.T.);
#4714=EDGE_CURVE('',#3612,#3787,#2262,.T.);
#4715=EDGE_CURVE('',#3722,#3607,#2263,.T.);
#4716=EDGE_CURVE('',#3606,#3723,#2264,.T.);
#4717=EDGE_CURVE('',#3728,#3601,#2265,.T.);
#4718=EDGE_CURVE('',#3600,#3729,#2266,.T.);
#4719=EDGE_CURVE('',#3734,#3595,#2267,.T.);
#4720=EDGE_CURVE('',#3594,#3735,#2268,.T.);
#4721=EDGE_CURVE('',#3740,#3589,#2269,.T.);
#4722=EDGE_CURVE('',#3588,#3741,#2270,.T.);
#4723=EDGE_CURVE('',#3746,#3583,#2271,.T.);
#4724=EDGE_CURVE('',#3582,#3747,#2272,.T.);
#4725=EDGE_CURVE('',#3752,#3577,#2273,.T.);
#4726=EDGE_CURVE('',#3576,#3753,#2274,.T.);
#4727=EDGE_CURVE('',#3758,#3571,#2275,.T.);
#4728=EDGE_CURVE('',#3570,#3759,#2276,.T.);
#4729=EDGE_CURVE('',#3764,#3565,#2277,.T.);
#4730=EDGE_CURVE('',#3564,#3765,#2278,.T.);
#4731=EDGE_CURVE('',#3770,#3559,#2279,.T.);
#4732=EDGE_CURVE('',#3558,#3771,#2280,.T.);
#4733=EDGE_CURVE('',#3787,#3788,#2281,.T.);
#4734=EDGE_CURVE('',#3788,#3789,#2282,.T.);
#4735=EDGE_CURVE('',#3789,#3790,#2283,.T.);
#4736=EDGE_CURVE('',#3790,#3782,#2284,.T.);
#4737=EDGE_CURVE('',#3790,#3791,#2285,.T.);
#4738=EDGE_CURVE('',#3783,#3791,#2286,.T.);
#4739=EDGE_CURVE('',#3792,#3793,#2287,.T.);
#4740=EDGE_CURVE('',#3794,#3792,#2288,.T.);
#4741=EDGE_CURVE('',#3794,#3795,#2289,.T.);
#4742=EDGE_CURVE('',#3793,#3795,#2290,.T.);
#4743=EDGE_CURVE('',#3796,#3786,#2291,.T.);
#4744=EDGE_CURVE('',#3788,#3796,#2292,.T.);
#4745=EDGE_CURVE('',#3797,#3796,#2293,.T.);
#4746=EDGE_CURVE('',#3789,#3797,#2294,.T.);
#4747=EDGE_CURVE('',#3795,#3797,#2295,.T.);
#4748=EDGE_CURVE('',#3791,#3794,#2296,.T.);
#4749=EDGE_CURVE('',#3798,#3792,#3396,.T.);
#4750=EDGE_CURVE('',#3799,#3798,#2297,.T.);
#4751=EDGE_CURVE('',#3800,#3799,#2298,.T.);
#4752=EDGE_CURVE('',#3801,#3800,#2299,.T.);
#4753=EDGE_CURVE('',#3802,#3801,#2300,.T.);
#4754=EDGE_CURVE('',#3803,#3802,#2301,.T.);
#4755=EDGE_CURVE('',#3804,#3803,#2302,.T.);
#4756=EDGE_CURVE('',#3784,#3804,#3397,.T.);
#4757=EDGE_CURVE('',#3805,#3793,#3398,.T.);
#4758=EDGE_CURVE('',#3805,#3798,#2303,.T.);
#4759=EDGE_CURVE('',#3804,#3806,#2304,.T.);
#4760=EDGE_CURVE('',#3803,#3807,#2305,.T.);
#4761=EDGE_CURVE('',#3806,#3807,#2306,.T.);
#4762=EDGE_CURVE('',#3808,#3805,#2307,.T.);
#4763=EDGE_CURVE('',#3799,#3808,#2308,.T.);
#4764=EDGE_CURVE('',#3809,#3808,#2309,.T.);
#4765=EDGE_CURVE('',#3800,#3809,#2310,.T.);
#4766=EDGE_CURVE('',#3810,#3809,#2311,.T.);
#4767=EDGE_CURVE('',#3801,#3810,#2312,.T.);
#4768=EDGE_CURVE('',#3811,#3810,#2313,.T.);
#4769=EDGE_CURVE('',#3802,#3811,#2314,.T.);
#4770=EDGE_CURVE('',#3807,#3811,#2315,.T.);
#4771=EDGE_CURVE('',#3785,#3806,#3399,.T.);
#4772=EDGE_CURVE('',#3812,#3812,#3400,.T.);
#4773=EDGE_CURVE('',#3812,#3813,#2316,.T.);
#4774=EDGE_CURVE('',#3813,#3813,#3401,.T.);
#4775=EDGE_CURVE('',#3814,#3814,#3402,.T.);
#4776=EDGE_CURVE('',#3815,#3815,#3403,.T.);
#4777=EDGE_CURVE('',#3816,#3816,#3404,.T.);
#4778=EDGE_CURVE('',#3816,#3815,#2317,.T.);
#4779=EDGE_CURVE('',#3817,#3817,#3405,.T.);
#4780=EDGE_CURVE('',#3818,#3818,#3406,.T.);
#4781=EDGE_CURVE('',#3817,#3819,#2318,.T.);
#4782=EDGE_CURVE('',#3819,#3819,#3407,.T.);
#4783=EDGE_CURVE('',#3814,#3818,#2319,.T.);
#4784=EDGE_CURVE('',#3820,#3821,#2320,.T.);
#4785=EDGE_CURVE('',#3822,#3820,#2321,.T.);
#4786=EDGE_CURVE('',#3823,#3822,#2322,.T.);
#4787=EDGE_CURVE('',#3821,#3823,#2323,.T.);
#4788=EDGE_CURVE('',#3824,#3825,#2324,.T.);
#4789=EDGE_CURVE('',#3826,#3824,#2325,.T.);
#4790=EDGE_CURVE('',#3827,#3826,#2326,.T.);
#4791=EDGE_CURVE('',#3825,#3827,#2327,.T.);
#4792=EDGE_CURVE('',#3822,#3827,#3408,.T.);
#4793=EDGE_CURVE('',#3825,#3820,#3409,.T.);
#4794=EDGE_CURVE('',#3824,#3821,#3410,.T.);
#4795=EDGE_CURVE('',#3823,#3826,#3411,.T.);
#4796=EDGE_CURVE('',#3828,#3829,#172,.T.);
#4797=EDGE_CURVE('',#3828,#3829,#3412,.T.);
#4798=EDGE_CURVE('',#3830,#3831,#173,.T.);
#4799=EDGE_CURVE('',#3830,#3831,#3413,.T.);
#4800=EDGE_CURVE('',#3832,#3833,#174,.T.);
#4801=EDGE_CURVE('',#3832,#3833,#3414,.T.);
#4802=EDGE_CURVE('',#3834,#3835,#175,.T.);
#4803=EDGE_CURVE('',#3834,#3835,#3415,.T.);
#4804=EDGE_CURVE('',#3836,#3831,#176,.T.);
#4805=EDGE_CURVE('',#3836,#3837,#177,.T.);
#4806=EDGE_CURVE('',#3838,#3837,#178,.T.);
#4807=EDGE_CURVE('',#3838,#3839,#179,.T.);
#4808=EDGE_CURVE('',#3830,#3839,#180,.T.);
#4809=EDGE_CURVE('',#3840,#3835,#181,.T.);
#4810=EDGE_CURVE('',#3840,#3841,#182,.T.);
#4811=EDGE_CURVE('',#3842,#3841,#183,.T.);
#4812=EDGE_CURVE('',#3842,#3843,#184,.T.);
#4813=EDGE_CURVE('',#3834,#3843,#185,.T.);
#4814=EDGE_CURVE('',#3828,#3844,#186,.T.);
#4815=EDGE_CURVE('',#3844,#3840,#2328,.T.);
#4816=EDGE_CURVE('',#3843,#3845,#2329,.T.);
#4817=EDGE_CURVE('',#3845,#3829,#187,.T.);
#4818=EDGE_CURVE('',#3846,#3846,#3416,.T.);
#4819=EDGE_CURVE('',#3847,#3847,#3417,.T.);
#4820=EDGE_CURVE('',#3848,#3848,#3418,.T.);
#4821=EDGE_CURVE('',#3849,#3849,#3419,.T.);
#4822=EDGE_CURVE('',#3849,#3846,#2330,.T.);
#4823=EDGE_CURVE('',#3850,#3850,#3420,.T.);
#4824=EDGE_CURVE('',#3850,#3851,#2331,.T.);
#4825=EDGE_CURVE('',#3851,#3851,#3421,.T.);
#4826=EDGE_CURVE('',#3852,#3852,#3422,.T.);
#4827=EDGE_CURVE('',#3852,#3853,#2332,.T.);
#4828=EDGE_CURVE('',#3853,#3853,#3423,.T.);
#4829=EDGE_CURVE('',#3854,#3854,#3424,.T.);
#4830=EDGE_CURVE('',#3854,#3847,#2333,.T.);
#4831=EDGE_CURVE('',#3855,#3855,#3425,.T.);
#4832=EDGE_CURVE('',#3855,#3856,#2334,.T.);
#4833=EDGE_CURVE('',#3856,#3856,#3426,.T.);
#4834=EDGE_CURVE('',#3857,#3857,#3427,.T.);
#4835=EDGE_CURVE('',#3858,#3858,#3428,.T.);
#4836=EDGE_CURVE('',#3858,#3859,#2335,.T.);
#4837=EDGE_CURVE('',#3859,#3859,#3429,.T.);
#4838=EDGE_CURVE('',#3860,#3860,#3430,.T.);
#4839=EDGE_CURVE('',#3857,#3861,#2336,.T.);
#4840=EDGE_CURVE('',#3861,#3861,#3431,.T.);
#4841=EDGE_CURVE('',#3860,#3862,#2337,.T.);
#4842=EDGE_CURVE('',#3862,#3862,#3432,.T.);
#4843=EDGE_CURVE('',#3863,#3864,#2338,.T.);
#4844=EDGE_CURVE('',#3865,#3863,#2339,.T.);
#4845=EDGE_CURVE('',#3866,#3865,#2340,.T.);
#4846=EDGE_CURVE('',#3866,#3864,#2341,.T.);
#4847=EDGE_CURVE('',#3867,#3868,#2342,.T.);
#4848=EDGE_CURVE('',#3867,#3869,#2343,.T.);
#4849=EDGE_CURVE('',#3870,#3869,#2344,.T.);
#4850=EDGE_CURVE('',#3868,#3870,#2345,.T.);
#4851=EDGE_CURVE('',#3871,#3872,#2346,.T.);
#4852=EDGE_CURVE('',#3871,#3873,#2347,.T.);
#4853=EDGE_CURVE('',#3874,#3873,#2348,.T.);
#4854=EDGE_CURVE('',#3872,#3874,#2349,.T.);
#4855=EDGE_CURVE('',#3875,#3876,#2350,.T.);
#4856=EDGE_CURVE('',#3875,#3877,#2351,.T.);
#4857=EDGE_CURVE('',#3878,#3877,#2352,.T.);
#4858=EDGE_CURVE('',#3876,#3878,#2353,.T.);
#4859=EDGE_CURVE('',#3879,#3880,#2354,.T.);
#4860=EDGE_CURVE('',#3879,#3881,#2355,.T.);
#4861=EDGE_CURVE('',#3882,#3881,#2356,.T.);
#4862=EDGE_CURVE('',#3880,#3882,#2357,.T.);
#4863=EDGE_CURVE('',#3883,#3884,#2358,.T.);
#4864=EDGE_CURVE('',#3885,#3883,#2359,.T.);
#4865=EDGE_CURVE('',#3886,#3885,#2360,.T.);
#4866=EDGE_CURVE('',#3886,#3884,#2361,.T.);
#4867=EDGE_CURVE('',#3887,#3888,#2362,.T.);
#4868=EDGE_CURVE('',#3889,#3887,#2363,.T.);
#4869=EDGE_CURVE('',#3890,#3889,#2364,.T.);
#4870=EDGE_CURVE('',#3890,#3888,#2365,.T.);
#4871=EDGE_CURVE('',#3891,#3891,#3433,.T.);
#4872=EDGE_CURVE('',#3892,#3892,#3434,.T.);
#4873=EDGE_CURVE('',#3864,#3879,#2366,.T.);
#4874=EDGE_CURVE('',#3881,#3866,#2367,.T.);
#4875=EDGE_CURVE('',#3884,#3867,#2368,.T.);
#4876=EDGE_CURVE('',#3869,#3886,#2369,.T.);
#4877=EDGE_CURVE('',#3888,#3871,#2370,.T.);
#4878=EDGE_CURVE('',#3873,#3890,#2371,.T.);
#4879=EDGE_CURVE('',#3893,#3875,#2372,.T.);
#4880=EDGE_CURVE('',#3894,#3893,#2373,.T.);
#4881=EDGE_CURVE('',#3877,#3894,#2374,.T.);
#4882=EDGE_CURVE('',#3895,#3893,#2375,.T.);
#4883=EDGE_CURVE('',#3896,#3895,#2376,.T.);
#4884=EDGE_CURVE('',#3894,#3896,#2377,.T.);
#4885=EDGE_CURVE('',#3897,#3898,#2378,.T.);
#4886=EDGE_CURVE('',#3899,#3898,#188,.T.);
#4887=EDGE_CURVE('',#3845,#3899,#189,.T.);
#4888=EDGE_CURVE('',#3897,#3842,#190,.T.);
#4889=EDGE_CURVE('',#3896,#3900,#2379,.T.);
#4890=EDGE_CURVE('',#3841,#3900,#191,.T.);
#4891=EDGE_CURVE('',#3901,#3844,#192,.T.);
#4892=EDGE_CURVE('',#3902,#3901,#193,.T.);
#4893=EDGE_CURVE('',#3902,#3878,#2380,.T.);
#4894=EDGE_CURVE('',#3889,#3903,#2381,.T.);
#4895=EDGE_CURVE('',#3904,#3903,#194,.T.);
#4896=EDGE_CURVE('',#3905,#3904,#195,.T.);
#4897=EDGE_CURVE('',#3906,#3905,#2382,.T.);
#4898=EDGE_CURVE('',#3907,#3906,#196,.T.);
#4899=EDGE_CURVE('',#3908,#3907,#197,.T.);
#4900=EDGE_CURVE('',#3908,#3874,#2383,.T.);
#4901=EDGE_CURVE('',#3885,#3909,#2384,.T.);
#4902=EDGE_CURVE('',#3837,#3909,#198,.T.);
#4903=EDGE_CURVE('',#3910,#3836,#2385,.T.);
#4904=EDGE_CURVE('',#3911,#3910,#199,.T.);
#4905=EDGE_CURVE('',#3912,#3911,#200,.T.);
#4906=EDGE_CURVE('',#3912,#3870,#2386,.T.);
#4907=EDGE_CURVE('',#3913,#3880,#2387,.T.);
#4908=EDGE_CURVE('',#3913,#3914,#201,.T.);
#4909=EDGE_CURVE('',#3914,#3915,#2388,.T.);
#4910=EDGE_CURVE('',#3915,#3916,#202,.T.);
#4911=EDGE_CURVE('',#3863,#3916,#2389,.T.);
#4912=EDGE_CURVE('',#3902,#3898,#203,.T.);
#4913=EDGE_CURVE('',#3897,#3900,#204,.T.);
#4914=EDGE_CURVE('',#3917,#3895,#2390,.T.);
#4915=EDGE_CURVE('',#3917,#3903,#205,.T.);
#4916=EDGE_CURVE('',#3918,#3887,#2391,.T.);
#4917=EDGE_CURVE('',#3918,#3909,#206,.T.);
#4918=EDGE_CURVE('',#3919,#3883,#2392,.T.);
#4919=EDGE_CURVE('',#3919,#3920,#207,.T.);
#4920=EDGE_CURVE('',#3920,#3913,#208,.T.);
#4921=EDGE_CURVE('',#3882,#3921,#2393,.T.);
#4922=EDGE_CURVE('',#3922,#3921,#209,.T.);
#4923=EDGE_CURVE('',#3922,#3923,#210,.T.);
#4924=EDGE_CURVE('',#3924,#3923,#211,.T.);
#4925=EDGE_CURVE('',#3924,#3925,#2394,.T.);
#4926=EDGE_CURVE('',#3926,#3925,#212,.T.);
#4927=EDGE_CURVE('',#3926,#3927,#213,.T.);
#4928=EDGE_CURVE('',#3928,#3927,#214,.T.);
#4929=EDGE_CURVE('',#3928,#3865,#2395,.T.);
#4930=EDGE_CURVE('',#3916,#3929,#215,.T.);
#4931=EDGE_CURVE('',#3929,#3930,#216,.T.);
#4932=EDGE_CURVE('',#3868,#3930,#2396,.T.);
#4933=EDGE_CURVE('',#3912,#3931,#217,.T.);
#4934=EDGE_CURVE('',#3872,#3931,#2397,.T.);
#4935=EDGE_CURVE('',#3908,#3932,#218,.T.);
#4936=EDGE_CURVE('',#3876,#3932,#2398,.T.);
#4937=EDGE_CURVE('',#3933,#3934,#219,.T.);
#4938=EDGE_CURVE('',#3934,#3935,#220,.T.);
#4939=EDGE_CURVE('',#3935,#3936,#2399,.T.);
#4940=EDGE_CURVE('',#3936,#3937,#221,.T.);
#4941=EDGE_CURVE('',#3937,#3938,#222,.T.);
#4942=EDGE_CURVE('',#3933,#3938,#2400,.T.);
#4943=EDGE_CURVE('',#3848,#3892,#2401,.T.);
#4944=EDGE_CURVE('',#3939,#3939,#3435,.T.);
#4945=EDGE_CURVE('',#3939,#3891,#2402,.T.);
#4946=EDGE_CURVE('',#3933,#3940,#223,.T.);
#4947=EDGE_CURVE('',#3941,#3938,#224,.T.);
#4948=EDGE_CURVE('',#3942,#3941,#225,.T.);
#4949=EDGE_CURVE('',#3943,#3942,#2403,.T.);
#4950=EDGE_CURVE('',#3940,#3943,#226,.T.);
#4951=EDGE_CURVE('',#3901,#3899,#227,.T.);
#4952=EDGE_CURVE('',#3940,#3944,#228,.T.);
#4953=EDGE_CURVE('',#3944,#3934,#229,.T.);
#4954=EDGE_CURVE('',#3945,#3943,#230,.T.);
#4955=EDGE_CURVE('',#3944,#3945,#3436,.F.);
#4956=EDGE_CURVE('',#3942,#3946,#231,.T.);
#4957=EDGE_CURVE('',#3946,#3945,#2404,.T.);
#4958=EDGE_CURVE('',#3937,#3947,#232,.T.);
#4959=EDGE_CURVE('',#3947,#3941,#233,.T.);
#4960=EDGE_CURVE('',#3948,#3932,#234,.T.);
#4961=EDGE_CURVE('',#3949,#3948,#235,.T.);
#4962=EDGE_CURVE('',#3950,#3949,#2405,.T.);
#4963=EDGE_CURVE('',#3951,#3950,#236,.T.);
#4964=EDGE_CURVE('',#3917,#3951,#237,.T.);
#4965=EDGE_CURVE('',#3907,#3948,#238,.T.);
#4966=EDGE_CURVE('',#3949,#3906,#239,.T.);
#4967=EDGE_CURVE('',#3905,#3950,#240,.T.);
#4968=EDGE_CURVE('',#3951,#3904,#241,.T.);
#4969=EDGE_CURVE('',#3952,#3931,#242,.T.);
#4970=EDGE_CURVE('',#3953,#3952,#243,.T.);
#4971=EDGE_CURVE('',#3839,#3953,#2406,.T.);
#4972=EDGE_CURVE('',#3918,#3838,#244,.T.);
#4973=EDGE_CURVE('',#3911,#3952,#245,.T.);
#4974=EDGE_CURVE('',#3953,#3833,#246,.T.);
#4975=EDGE_CURVE('',#3832,#3910,#247,.T.);
#4976=EDGE_CURVE('',#3954,#3930,#248,.T.);
#4977=EDGE_CURVE('',#3955,#3954,#249,.T.);
#4978=EDGE_CURVE('',#3956,#3955,#2407,.T.);
#4979=EDGE_CURVE('',#3957,#3956,#250,.T.);
#4980=EDGE_CURVE('',#3919,#3957,#251,.T.);
#4981=EDGE_CURVE('',#3929,#3958,#252,.T.);
#4982=EDGE_CURVE('',#3958,#3954,#253,.T.);
#4983=EDGE_CURVE('',#3959,#3958,#3437,.F.);
#4984=EDGE_CURVE('',#3955,#3959,#254,.T.);
#4985=EDGE_CURVE('',#3959,#3960,#2408,.T.);
#4986=EDGE_CURVE('',#3960,#3956,#255,.T.);
#4987=EDGE_CURVE('',#3957,#3961,#256,.T.);
#4988=EDGE_CURVE('',#3961,#3920,#257,.T.);
#4989=EDGE_CURVE('',#3961,#3960,#3438,.F.);
#4990=EDGE_CURVE('',#3960,#3914,#3439,.F.);
#4991=EDGE_CURVE('',#3914,#3961,#3440,.F.);
#4992=EDGE_CURVE('',#3946,#3947,#3441,.F.);
#4993=EDGE_CURVE('',#3947,#3962,#3442,.F.);
#4994=EDGE_CURVE('',#3962,#3946,#3443,.F.);
#4995=EDGE_CURVE('',#3958,#3915,#3444,.F.);
#4996=EDGE_CURVE('',#3915,#3959,#3445,.F.);
#4997=EDGE_CURVE('',#3963,#3944,#3446,.F.);
#4998=EDGE_CURVE('',#3945,#3963,#3447,.F.);
#4999=EDGE_CURVE('',#3963,#3962,#2409,.T.);
#5000=EDGE_CURVE('',#3935,#3963,#258,.T.);
#5001=EDGE_CURVE('',#3962,#3936,#259,.T.);
#5002=EDGE_CURVE('',#3964,#3965,#3448,.F.);
#5003=EDGE_CURVE('',#3966,#3964,#3449,.F.);
#5004=EDGE_CURVE('',#3965,#3966,#3450,.F.);
#5005=EDGE_CURVE('',#3967,#3968,#3451,.F.);
#5006=EDGE_CURVE('',#3969,#3967,#3452,.F.);
#5007=EDGE_CURVE('',#3968,#3969,#3453,.F.);
#5008=EDGE_CURVE('',#3970,#3971,#3454,.F.);
#5009=EDGE_CURVE('',#3972,#3970,#3455,.F.);
#5010=EDGE_CURVE('',#3971,#3972,#3456,.F.);
#5011=EDGE_CURVE('',#3965,#3972,#2410,.T.);
#5012=EDGE_CURVE('',#3970,#3964,#2411,.T.);
#5013=EDGE_CURVE('',#3927,#3971,#260,.T.);
#5014=EDGE_CURVE('',#3972,#3928,#261,.T.);
#5015=EDGE_CURVE('',#3973,#3974,#3457,.F.);
#5016=EDGE_CURVE('',#3975,#3973,#3458,.F.);
#5017=EDGE_CURVE('',#3974,#3975,#3459,.F.);
#5018=EDGE_CURVE('',#3973,#3969,#2412,.T.);
#5019=EDGE_CURVE('',#3967,#3975,#2413,.T.);
#5020=EDGE_CURVE('',#3971,#3974,#262,.T.);
#5021=EDGE_CURVE('',#3975,#3970,#263,.T.);
#5022=EDGE_CURVE('',#3925,#3973,#264,.T.);
#5023=EDGE_CURVE('',#3974,#3926,#265,.T.);
#5024=EDGE_CURVE('',#3923,#3968,#266,.T.);
#5025=EDGE_CURVE('',#3969,#3924,#267,.T.);
#5026=EDGE_CURVE('',#3968,#3966,#268,.T.);
#5027=EDGE_CURVE('',#3964,#3967,#269,.T.);
#5028=EDGE_CURVE('',#3921,#3965,#270,.T.);
#5029=EDGE_CURVE('',#3966,#3922,#271,.T.);
#5030=EDGE_CURVE('',#3976,#3977,#272,.T.);
#5031=EDGE_CURVE('',#3976,#3977,#3460,.T.);
#5032=EDGE_CURVE('',#3978,#3979,#273,.T.);
#5033=EDGE_CURVE('',#3978,#3979,#3461,.T.);
#5034=EDGE_CURVE('',#3980,#3981,#274,.T.);
#5035=EDGE_CURVE('',#3980,#3981,#3462,.T.);
#5036=EDGE_CURVE('',#3982,#3983,#275,.T.);
#5037=EDGE_CURVE('',#3982,#3983,#3463,.T.);
#5038=EDGE_CURVE('',#3984,#3979,#276,.T.);
#5039=EDGE_CURVE('',#3984,#3985,#277,.T.);
#5040=EDGE_CURVE('',#3986,#3985,#278,.T.);
#5041=EDGE_CURVE('',#3986,#3987,#279,.T.);
#5042=EDGE_CURVE('',#3978,#3987,#280,.T.);
#5043=EDGE_CURVE('',#3988,#3983,#281,.T.);
#5044=EDGE_CURVE('',#3988,#3989,#282,.T.);
#5045=EDGE_CURVE('',#3990,#3989,#283,.T.);
#5046=EDGE_CURVE('',#3990,#3991,#284,.T.);
#5047=EDGE_CURVE('',#3982,#3991,#285,.T.);
#5048=EDGE_CURVE('',#3976,#3992,#286,.T.);
#5049=EDGE_CURVE('',#3992,#3988,#2414,.T.);
#5050=EDGE_CURVE('',#3991,#3993,#2415,.T.);
#5051=EDGE_CURVE('',#3993,#3977,#287,.T.);
#5052=EDGE_CURVE('',#3994,#3994,#3464,.T.);
#5053=EDGE_CURVE('',#3995,#3995,#3465,.T.);
#5054=EDGE_CURVE('',#3996,#3996,#3466,.T.);
#5055=EDGE_CURVE('',#3997,#3998,#2416,.T.);
#5056=EDGE_CURVE('',#3997,#3999,#2417,.T.);
#5057=EDGE_CURVE('',#3999,#4000,#2418,.T.);
#5058=EDGE_CURVE('',#3998,#4000,#2419,.T.);
#5059=EDGE_CURVE('',#4001,#3997,#2420,.T.);
#5060=EDGE_CURVE('',#4001,#4002,#2421,.T.);
#5061=EDGE_CURVE('',#4002,#3999,#2422,.T.);
#5062=EDGE_CURVE('',#4003,#4001,#2423,.T.);
#5063=EDGE_CURVE('',#4003,#4004,#2424,.T.);
#5064=EDGE_CURVE('',#4004,#4002,#2425,.T.);
#5065=EDGE_CURVE('',#4005,#4003,#2426,.T.);
#5066=EDGE_CURVE('',#4005,#4006,#2427,.T.);
#5067=EDGE_CURVE('',#4006,#4004,#2428,.T.);
#5068=EDGE_CURVE('',#4007,#4005,#2429,.T.);
#5069=EDGE_CURVE('',#4007,#4008,#2430,.T.);
#5070=EDGE_CURVE('',#4008,#4006,#2431,.T.);
#5071=EDGE_CURVE('',#3998,#4007,#2432,.T.);
#5072=EDGE_CURVE('',#4000,#4008,#2433,.T.);
#5073=EDGE_CURVE('',#4009,#4009,#3467,.T.);
#5074=EDGE_CURVE('',#4010,#4011,#2434,.T.);
#5075=EDGE_CURVE('',#4010,#4012,#2435,.T.);
#5076=EDGE_CURVE('',#4012,#4013,#2436,.T.);
#5077=EDGE_CURVE('',#4011,#4013,#2437,.T.);
#5078=EDGE_CURVE('',#4014,#4010,#2438,.T.);
#5079=EDGE_CURVE('',#4014,#4015,#2439,.T.);
#5080=EDGE_CURVE('',#4015,#4012,#2440,.T.);
#5081=EDGE_CURVE('',#4016,#4014,#2441,.T.);
#5082=EDGE_CURVE('',#4016,#4017,#2442,.T.);
#5083=EDGE_CURVE('',#4017,#4015,#2443,.T.);
#5084=EDGE_CURVE('',#4018,#4016,#2444,.T.);
#5085=EDGE_CURVE('',#4018,#4019,#2445,.T.);
#5086=EDGE_CURVE('',#4019,#4017,#2446,.T.);
#5087=EDGE_CURVE('',#4020,#4018,#2447,.T.);
#5088=EDGE_CURVE('',#4020,#4021,#2448,.T.);
#5089=EDGE_CURVE('',#4021,#4019,#2449,.T.);
#5090=EDGE_CURVE('',#4011,#4020,#2450,.T.);
#5091=EDGE_CURVE('',#4013,#4021,#2451,.T.);
#5092=EDGE_CURVE('',#4022,#4022,#3468,.T.);
#5093=EDGE_CURVE('',#4023,#4023,#3469,.T.);
#5094=EDGE_CURVE('',#4023,#3994,#2452,.T.);
#5095=EDGE_CURVE('',#4024,#4024,#3470,.T.);
#5096=EDGE_CURVE('',#4024,#4025,#2453,.T.);
#5097=EDGE_CURVE('',#4025,#4025,#3471,.T.);
#5098=EDGE_CURVE('',#4026,#4026,#3472,.T.);
#5099=EDGE_CURVE('',#4026,#4027,#2454,.T.);
#5100=EDGE_CURVE('',#4027,#4027,#3473,.T.);
#5101=EDGE_CURVE('',#4028,#4028,#3474,.T.);
#5102=EDGE_CURVE('',#4028,#3995,#2455,.T.);
#5103=EDGE_CURVE('',#4022,#4029,#2456,.T.);
#5104=EDGE_CURVE('',#4029,#4029,#3475,.T.);
#5105=EDGE_CURVE('',#4009,#4030,#2457,.T.);
#5106=EDGE_CURVE('',#4030,#4030,#3476,.T.);
#5107=EDGE_CURVE('',#4031,#4032,#2458,.T.);
#5108=EDGE_CURVE('',#4033,#4031,#2459,.T.);
#5109=EDGE_CURVE('',#4034,#4033,#2460,.T.);
#5110=EDGE_CURVE('',#4034,#4032,#2461,.T.);
#5111=EDGE_CURVE('',#4035,#4036,#2462,.T.);
#5112=EDGE_CURVE('',#4035,#4037,#2463,.T.);
#5113=EDGE_CURVE('',#4038,#4037,#2464,.T.);
#5114=EDGE_CURVE('',#4036,#4038,#2465,.T.);
#5115=EDGE_CURVE('',#4039,#4040,#2466,.T.);
#5116=EDGE_CURVE('',#4039,#4041,#2467,.T.);
#5117=EDGE_CURVE('',#4042,#4041,#2468,.T.);
#5118=EDGE_CURVE('',#4040,#4042,#2469,.T.);
#5119=EDGE_CURVE('',#4043,#4044,#2470,.T.);
#5120=EDGE_CURVE('',#4043,#4045,#2471,.T.);
#5121=EDGE_CURVE('',#4046,#4045,#2472,.T.);
#5122=EDGE_CURVE('',#4044,#4046,#2473,.T.);
#5123=EDGE_CURVE('',#4047,#4048,#2474,.T.);
#5124=EDGE_CURVE('',#4047,#4049,#2475,.T.);
#5125=EDGE_CURVE('',#4050,#4049,#2476,.T.);
#5126=EDGE_CURVE('',#4048,#4050,#2477,.T.);
#5127=EDGE_CURVE('',#4051,#4052,#2478,.T.);
#5128=EDGE_CURVE('',#4053,#4051,#2479,.T.);
#5129=EDGE_CURVE('',#4054,#4053,#2480,.T.);
#5130=EDGE_CURVE('',#4054,#4052,#2481,.T.);
#5131=EDGE_CURVE('',#4055,#4056,#2482,.T.);
#5132=EDGE_CURVE('',#4057,#4055,#2483,.T.);
#5133=EDGE_CURVE('',#4058,#4057,#2484,.T.);
#5134=EDGE_CURVE('',#4058,#4056,#2485,.T.);
#5135=EDGE_CURVE('',#4059,#4059,#3477,.T.);
#5136=EDGE_CURVE('',#4060,#4060,#3478,.T.);
#5137=EDGE_CURVE('',#4032,#4047,#2486,.T.);
#5138=EDGE_CURVE('',#4049,#4034,#2487,.T.);
#5139=EDGE_CURVE('',#4052,#4035,#2488,.T.);
#5140=EDGE_CURVE('',#4037,#4054,#2489,.T.);
#5141=EDGE_CURVE('',#4056,#4039,#2490,.T.);
#5142=EDGE_CURVE('',#4041,#4058,#2491,.T.);
#5143=EDGE_CURVE('',#4061,#4043,#2492,.T.);
#5144=EDGE_CURVE('',#4062,#4061,#2493,.T.);
#5145=EDGE_CURVE('',#4045,#4062,#2494,.T.);
#5146=EDGE_CURVE('',#4063,#4061,#2495,.T.);
#5147=EDGE_CURVE('',#4064,#4063,#2496,.T.);
#5148=EDGE_CURVE('',#4062,#4064,#2497,.T.);
#5149=EDGE_CURVE('',#4065,#4066,#2498,.T.);
#5150=EDGE_CURVE('',#4067,#4066,#288,.T.);
#5151=EDGE_CURVE('',#3993,#4067,#289,.T.);
#5152=EDGE_CURVE('',#4065,#3990,#290,.T.);
#5153=EDGE_CURVE('',#4064,#4068,#2499,.T.);
#5154=EDGE_CURVE('',#3989,#4068,#291,.T.);
#5155=EDGE_CURVE('',#4069,#3992,#292,.T.);
#5156=EDGE_CURVE('',#4070,#4069,#293,.T.);
#5157=EDGE_CURVE('',#4070,#4046,#2500,.T.);
#5158=EDGE_CURVE('',#4057,#4071,#2501,.T.);
#5159=EDGE_CURVE('',#4072,#4071,#294,.T.);
#5160=EDGE_CURVE('',#4073,#4072,#295,.T.);
#5161=EDGE_CURVE('',#4074,#4073,#2502,.T.);
#5162=EDGE_CURVE('',#4075,#4074,#296,.T.);
#5163=EDGE_CURVE('',#4076,#4075,#297,.T.);
#5164=EDGE_CURVE('',#4076,#4042,#2503,.T.);
#5165=EDGE_CURVE('',#4053,#4077,#2504,.T.);
#5166=EDGE_CURVE('',#3985,#4077,#298,.T.);
#5167=EDGE_CURVE('',#4078,#3984,#2505,.T.);
#5168=EDGE_CURVE('',#4079,#4078,#299,.T.);
#5169=EDGE_CURVE('',#4080,#4079,#300,.T.);
#5170=EDGE_CURVE('',#4080,#4038,#2506,.T.);
#5171=EDGE_CURVE('',#4081,#4048,#2507,.T.);
#5172=EDGE_CURVE('',#4081,#4082,#301,.T.);
#5173=EDGE_CURVE('',#4082,#4083,#2508,.T.);
#5174=EDGE_CURVE('',#4083,#4084,#302,.T.);
#5175=EDGE_CURVE('',#4031,#4084,#2509,.T.);
#5176=EDGE_CURVE('',#4070,#4066,#303,.T.);
#5177=EDGE_CURVE('',#4065,#4068,#304,.T.);
#5178=EDGE_CURVE('',#4085,#4063,#2510,.T.);
#5179=EDGE_CURVE('',#4085,#4071,#305,.T.);
#5180=EDGE_CURVE('',#4086,#4055,#2511,.T.);
#5181=EDGE_CURVE('',#4086,#4077,#306,.T.);
#5182=EDGE_CURVE('',#4087,#4051,#2512,.T.);
#5183=EDGE_CURVE('',#4087,#4088,#307,.T.);
#5184=EDGE_CURVE('',#4088,#4081,#308,.T.);
#5185=EDGE_CURVE('',#4050,#4089,#2513,.T.);
#5186=EDGE_CURVE('',#4090,#4089,#309,.T.);
#5187=EDGE_CURVE('',#4090,#4091,#310,.T.);
#5188=EDGE_CURVE('',#4092,#4091,#311,.T.);
#5189=EDGE_CURVE('',#4092,#4093,#2514,.T.);
#5190=EDGE_CURVE('',#4094,#4093,#312,.T.);
#5191=EDGE_CURVE('',#4094,#4095,#313,.T.);
#5192=EDGE_CURVE('',#4096,#4095,#314,.T.);
#5193=EDGE_CURVE('',#4096,#4033,#2515,.T.);
#5194=EDGE_CURVE('',#4084,#4097,#315,.T.);
#5195=EDGE_CURVE('',#4097,#4098,#316,.T.);
#5196=EDGE_CURVE('',#4036,#4098,#2516,.T.);
#5197=EDGE_CURVE('',#4080,#4099,#317,.T.);
#5198=EDGE_CURVE('',#4040,#4099,#2517,.T.);
#5199=EDGE_CURVE('',#4076,#4100,#318,.T.);
#5200=EDGE_CURVE('',#4044,#4100,#2518,.T.);
#5201=EDGE_CURVE('',#4101,#4102,#319,.T.);
#5202=EDGE_CURVE('',#4102,#4103,#320,.T.);
#5203=EDGE_CURVE('',#4103,#4104,#2519,.T.);
#5204=EDGE_CURVE('',#4104,#4105,#321,.T.);
#5205=EDGE_CURVE('',#4105,#4106,#322,.T.);
#5206=EDGE_CURVE('',#4101,#4106,#2520,.T.);
#5207=EDGE_CURVE('',#3996,#4060,#2521,.T.);
#5208=EDGE_CURVE('',#4107,#4107,#3479,.T.);
#5209=EDGE_CURVE('',#4107,#4059,#2522,.T.);
#5210=EDGE_CURVE('',#4101,#4108,#323,.T.);
#5211=EDGE_CURVE('',#4109,#4106,#324,.T.);
#5212=EDGE_CURVE('',#4110,#4109,#325,.T.);
#5213=EDGE_CURVE('',#4111,#4110,#2523,.T.);
#5214=EDGE_CURVE('',#4108,#4111,#326,.T.);
#5215=EDGE_CURVE('',#4069,#4067,#327,.T.);
#5216=EDGE_CURVE('',#4108,#4112,#328,.T.);
#5217=EDGE_CURVE('',#4112,#4102,#329,.T.);
#5218=EDGE_CURVE('',#4113,#4111,#330,.T.);
#5219=EDGE_CURVE('',#4112,#4113,#3480,.F.);
#5220=EDGE_CURVE('',#4110,#4114,#331,.T.);
#5221=EDGE_CURVE('',#4114,#4113,#2524,.T.);
#5222=EDGE_CURVE('',#4105,#4115,#332,.T.);
#5223=EDGE_CURVE('',#4115,#4109,#333,.T.);
#5224=EDGE_CURVE('',#4116,#4100,#334,.T.);
#5225=EDGE_CURVE('',#4117,#4116,#335,.T.);
#5226=EDGE_CURVE('',#4118,#4117,#2525,.T.);
#5227=EDGE_CURVE('',#4119,#4118,#336,.T.);
#5228=EDGE_CURVE('',#4085,#4119,#337,.T.);
#5229=EDGE_CURVE('',#4075,#4116,#338,.T.);
#5230=EDGE_CURVE('',#4117,#4074,#339,.T.);
#5231=EDGE_CURVE('',#4073,#4118,#340,.T.);
#5232=EDGE_CURVE('',#4119,#4072,#341,.T.);
#5233=EDGE_CURVE('',#4120,#4099,#342,.T.);
#5234=EDGE_CURVE('',#4121,#4120,#343,.T.);
#5235=EDGE_CURVE('',#3987,#4121,#2526,.T.);
#5236=EDGE_CURVE('',#4086,#3986,#344,.T.);
#5237=EDGE_CURVE('',#4079,#4120,#345,.T.);
#5238=EDGE_CURVE('',#4121,#3981,#346,.T.);
#5239=EDGE_CURVE('',#3980,#4078,#347,.T.);
#5240=EDGE_CURVE('',#4122,#4098,#348,.T.);
#5241=EDGE_CURVE('',#4123,#4122,#349,.T.);
#5242=EDGE_CURVE('',#4124,#4123,#2527,.T.);
#5243=EDGE_CURVE('',#4125,#4124,#350,.T.);
#5244=EDGE_CURVE('',#4087,#4125,#351,.T.);
#5245=EDGE_CURVE('',#4097,#4126,#352,.T.);
#5246=EDGE_CURVE('',#4126,#4122,#353,.T.);
#5247=EDGE_CURVE('',#4127,#4126,#3481,.F.);
#5248=EDGE_CURVE('',#4123,#4127,#354,.T.);
#5249=EDGE_CURVE('',#4127,#4128,#2528,.T.);
#5250=EDGE_CURVE('',#4128,#4124,#355,.T.);
#5251=EDGE_CURVE('',#4125,#4129,#356,.T.);
#5252=EDGE_CURVE('',#4129,#4088,#357,.T.);
#5253=EDGE_CURVE('',#4129,#4128,#3482,.F.);
#5254=EDGE_CURVE('',#4128,#4082,#3483,.F.);
#5255=EDGE_CURVE('',#4082,#4129,#3484,.F.);
#5256=EDGE_CURVE('',#4114,#4115,#3485,.F.);
#5257=EDGE_CURVE('',#4115,#4130,#3486,.F.);
#5258=EDGE_CURVE('',#4130,#4114,#3487,.F.);
#5259=EDGE_CURVE('',#4126,#4083,#3488,.F.);
#5260=EDGE_CURVE('',#4083,#4127,#3489,.F.);
#5261=EDGE_CURVE('',#4131,#4112,#3490,.F.);
#5262=EDGE_CURVE('',#4113,#4131,#3491,.F.);
#5263=EDGE_CURVE('',#4131,#4130,#2529,.T.);
#5264=EDGE_CURVE('',#4103,#4131,#358,.T.);
#5265=EDGE_CURVE('',#4130,#4104,#359,.T.);
#5266=EDGE_CURVE('',#4132,#4133,#3492,.F.);
#5267=EDGE_CURVE('',#4134,#4132,#3493,.F.);
#5268=EDGE_CURVE('',#4133,#4134,#3494,.F.);
#5269=EDGE_CURVE('',#4135,#4136,#3495,.F.);
#5270=EDGE_CURVE('',#4137,#4135,#3496,.F.);
#5271=EDGE_CURVE('',#4136,#4137,#3497,.F.);
#5272=EDGE_CURVE('',#4138,#4139,#3498,.F.);
#5273=EDGE_CURVE('',#4140,#4138,#3499,.F.);
#5274=EDGE_CURVE('',#4139,#4140,#3500,.F.);
#5275=EDGE_CURVE('',#4133,#4140,#2530,.T.);
#5276=EDGE_CURVE('',#4138,#4132,#2531,.T.);
#5277=EDGE_CURVE('',#4095,#4139,#360,.T.);
#5278=EDGE_CURVE('',#4140,#4096,#361,.T.);
#5279=EDGE_CURVE('',#4141,#4142,#3501,.F.);
#5280=EDGE_CURVE('',#4143,#4141,#3502,.F.);
#5281=EDGE_CURVE('',#4142,#4143,#3503,.F.);
#5282=EDGE_CURVE('',#4141,#4137,#2532,.T.);
#5283=EDGE_CURVE('',#4135,#4143,#2533,.T.);
#5284=EDGE_CURVE('',#4139,#4142,#362,.T.);
#5285=EDGE_CURVE('',#4143,#4138,#363,.T.);
#5286=EDGE_CURVE('',#4093,#4141,#364,.T.);
#5287=EDGE_CURVE('',#4142,#4094,#365,.T.);
#5288=EDGE_CURVE('',#4091,#4136,#366,.T.);
#5289=EDGE_CURVE('',#4137,#4092,#367,.T.);
#5290=EDGE_CURVE('',#4136,#4134,#368,.T.);
#5291=EDGE_CURVE('',#4132,#4135,#369,.T.);
#5292=EDGE_CURVE('',#4089,#4133,#370,.T.);
#5293=EDGE_CURVE('',#4134,#4090,#371,.T.);
#5294=EDGE_CURVE('',#4144,#4145,#2534,.T.);
#5295=EDGE_CURVE('',#4144,#4146,#372,.T.);
#5296=EDGE_CURVE('',#4146,#4147,#3504,.F.);
#5297=EDGE_CURVE('',#4147,#4145,#373,.T.);
#5298=EDGE_CURVE('',#4148,#4149,#2535,.T.);
#5299=EDGE_CURVE('',#4148,#4144,#374,.T.);
#5300=EDGE_CURVE('',#4145,#4149,#375,.T.);
#5301=EDGE_CURVE('',#4150,#4151,#2536,.T.);
#5302=EDGE_CURVE('',#4150,#4148,#376,.T.);
#5303=EDGE_CURVE('',#4149,#4151,#377,.T.);
#5304=EDGE_CURVE('',#4152,#4153,#2537,.T.);
#5305=EDGE_CURVE('',#4152,#4150,#378,.T.);
#5306=EDGE_CURVE('',#4151,#4153,#379,.T.);
#5307=EDGE_CURVE('',#4154,#4155,#2538,.T.);
#5308=EDGE_CURVE('',#4154,#4152,#380,.T.);
#5309=EDGE_CURVE('',#4153,#4155,#381,.T.);
#5310=EDGE_CURVE('',#4156,#4157,#2539,.T.);
#5311=EDGE_CURVE('',#4156,#4154,#382,.T.);
#5312=EDGE_CURVE('',#4155,#4157,#383,.T.);
#5313=EDGE_CURVE('',#4158,#4159,#2540,.T.);
#5314=EDGE_CURVE('',#4158,#4156,#384,.T.);
#5315=EDGE_CURVE('',#4157,#4159,#385,.T.);
#5316=EDGE_CURVE('',#4160,#4161,#2541,.T.);
#5317=EDGE_CURVE('',#4160,#4158,#386,.T.);
#5318=EDGE_CURVE('',#4159,#4161,#387,.T.);
#5319=EDGE_CURVE('',#4162,#4163,#2542,.T.);
#5320=EDGE_CURVE('',#4162,#4160,#388,.T.);
#5321=EDGE_CURVE('',#4161,#4163,#389,.T.);
#5322=EDGE_CURVE('',#4164,#4165,#2543,.T.);
#5323=EDGE_CURVE('',#4164,#4162,#390,.T.);
#5324=EDGE_CURVE('',#4163,#4165,#391,.T.);
#5325=EDGE_CURVE('',#4166,#4167,#2544,.T.);
#5326=EDGE_CURVE('',#4166,#4164,#392,.T.);
#5327=EDGE_CURVE('',#4165,#4167,#393,.T.);
#5328=EDGE_CURVE('',#4168,#4169,#2545,.T.);
#5329=EDGE_CURVE('',#4168,#4166,#394,.T.);
#5330=EDGE_CURVE('',#4167,#4169,#395,.T.);
#5331=EDGE_CURVE('',#4170,#4171,#2546,.T.);
#5332=EDGE_CURVE('',#4170,#4168,#396,.T.);
#5333=EDGE_CURVE('',#4169,#4171,#397,.T.);
#5334=EDGE_CURVE('',#4172,#4173,#2547,.T.);
#5335=EDGE_CURVE('',#4172,#4170,#398,.T.);
#5336=EDGE_CURVE('',#4171,#4173,#399,.T.);
#5337=EDGE_CURVE('',#4174,#4175,#2548,.T.);
#5338=EDGE_CURVE('',#4174,#4172,#400,.T.);
#5339=EDGE_CURVE('',#4173,#4175,#401,.T.);
#5340=EDGE_CURVE('',#4176,#4177,#2549,.T.);
#5341=EDGE_CURVE('',#4176,#4174,#402,.T.);
#5342=EDGE_CURVE('',#4175,#4177,#403,.T.);
#5343=EDGE_CURVE('',#4178,#4179,#2550,.T.);
#5344=EDGE_CURVE('',#4178,#4176,#404,.T.);
#5345=EDGE_CURVE('',#4177,#4179,#405,.T.);
#5346=EDGE_CURVE('',#4180,#4181,#2551,.T.);
#5347=EDGE_CURVE('',#4180,#4178,#406,.T.);
#5348=EDGE_CURVE('',#4179,#4181,#407,.T.);
#5349=EDGE_CURVE('',#4182,#4183,#2552,.T.);
#5350=EDGE_CURVE('',#4182,#4180,#408,.T.);
#5351=EDGE_CURVE('',#4181,#4183,#409,.T.);
#5352=EDGE_CURVE('',#4184,#4185,#2553,.T.);
#5353=EDGE_CURVE('',#4184,#4182,#410,.T.);
#5354=EDGE_CURVE('',#4183,#4185,#411,.T.);
#5355=EDGE_CURVE('',#4186,#4187,#2554,.T.);
#5356=EDGE_CURVE('',#4186,#4184,#412,.T.);
#5357=EDGE_CURVE('',#4185,#4187,#413,.T.);
#5358=EDGE_CURVE('',#4188,#4189,#2555,.T.);
#5359=EDGE_CURVE('',#4188,#4186,#414,.T.);
#5360=EDGE_CURVE('',#4187,#4189,#415,.T.);
#5361=EDGE_CURVE('',#4190,#4191,#2556,.T.);
#5362=EDGE_CURVE('',#4190,#4188,#416,.T.);
#5363=EDGE_CURVE('',#4189,#4191,#417,.T.);
#5364=EDGE_CURVE('',#4192,#4193,#2557,.T.);
#5365=EDGE_CURVE('',#4192,#4190,#418,.T.);
#5366=EDGE_CURVE('',#4191,#4193,#419,.T.);
#5367=EDGE_CURVE('',#4194,#4195,#2558,.T.);
#5368=EDGE_CURVE('',#4194,#4192,#420,.T.);
#5369=EDGE_CURVE('',#4193,#4195,#421,.T.);
#5370=EDGE_CURVE('',#4196,#4197,#2559,.T.);
#5371=EDGE_CURVE('',#4196,#4194,#422,.T.);
#5372=EDGE_CURVE('',#4195,#4197,#423,.T.);
#5373=EDGE_CURVE('',#4198,#4199,#2560,.T.);
#5374=EDGE_CURVE('',#4198,#4196,#424,.T.);
#5375=EDGE_CURVE('',#4197,#4199,#425,.T.);
#5376=EDGE_CURVE('',#4200,#4201,#2561,.T.);
#5377=EDGE_CURVE('',#4200,#4198,#426,.T.);
#5378=EDGE_CURVE('',#4199,#4201,#427,.T.);
#5379=EDGE_CURVE('',#4202,#4203,#2562,.T.);
#5380=EDGE_CURVE('',#4202,#4200,#428,.T.);
#5381=EDGE_CURVE('',#4201,#4203,#429,.T.);
#5382=EDGE_CURVE('',#4204,#4205,#2563,.T.);
#5383=EDGE_CURVE('',#4204,#4202,#430,.T.);
#5384=EDGE_CURVE('',#4203,#4205,#431,.T.);
#5385=EDGE_CURVE('',#4206,#4207,#2564,.T.);
#5386=EDGE_CURVE('',#4206,#4208,#432,.T.);
#5387=EDGE_CURVE('',#4208,#4209,#3505,.T.);
#5388=EDGE_CURVE('',#4207,#4209,#433,.T.);
#5389=EDGE_CURVE('',#4210,#4211,#2565,.T.);
#5390=EDGE_CURVE('',#4210,#4206,#434,.T.);
#5391=EDGE_CURVE('',#4211,#4207,#435,.T.);
#5392=EDGE_CURVE('',#4212,#4213,#2566,.T.);
#5393=EDGE_CURVE('',#4212,#4210,#436,.T.);
#5394=EDGE_CURVE('',#4213,#4211,#437,.T.);
#5395=EDGE_CURVE('',#4214,#4215,#2567,.T.);
#5396=EDGE_CURVE('',#4214,#4212,#438,.T.);
#5397=EDGE_CURVE('',#4215,#4213,#439,.T.);
#5398=EDGE_CURVE('',#4216,#4217,#2568,.T.);
#5399=EDGE_CURVE('',#4216,#4214,#440,.T.);
#5400=EDGE_CURVE('',#4217,#4215,#441,.T.);
#5401=EDGE_CURVE('',#4218,#4219,#2569,.T.);
#5402=EDGE_CURVE('',#4218,#4216,#442,.T.);
#5403=EDGE_CURVE('',#4219,#4217,#443,.T.);
#5404=EDGE_CURVE('',#4220,#4221,#2570,.T.);
#5405=EDGE_CURVE('',#4220,#4218,#444,.T.);
#5406=EDGE_CURVE('',#4221,#4219,#445,.T.);
#5407=EDGE_CURVE('',#4222,#4223,#2571,.T.);
#5408=EDGE_CURVE('',#4222,#4220,#446,.T.);
#5409=EDGE_CURVE('',#4223,#4221,#447,.T.);
#5410=EDGE_CURVE('',#4224,#4225,#2572,.T.);
#5411=EDGE_CURVE('',#4224,#4222,#448,.T.);
#5412=EDGE_CURVE('',#4225,#4223,#449,.T.);
#5413=EDGE_CURVE('',#4226,#4227,#2573,.T.);
#5414=EDGE_CURVE('',#4226,#4224,#450,.T.);
#5415=EDGE_CURVE('',#4227,#4225,#451,.T.);
#5416=EDGE_CURVE('',#4228,#4229,#2574,.T.);
#5417=EDGE_CURVE('',#4228,#4226,#452,.T.);
#5418=EDGE_CURVE('',#4229,#4227,#453,.T.);
#5419=EDGE_CURVE('',#4230,#4231,#2575,.T.);
#5420=EDGE_CURVE('',#4230,#4228,#454,.T.);
#5421=EDGE_CURVE('',#4231,#4229,#455,.T.);
#5422=EDGE_CURVE('',#4232,#4233,#2576,.T.);
#5423=EDGE_CURVE('',#4232,#4230,#456,.T.);
#5424=EDGE_CURVE('',#4233,#4231,#457,.T.);
#5425=EDGE_CURVE('',#4234,#4235,#2577,.T.);
#5426=EDGE_CURVE('',#4234,#4232,#458,.T.);
#5427=EDGE_CURVE('',#4235,#4233,#459,.T.);
#5428=EDGE_CURVE('',#4236,#4237,#2578,.T.);
#5429=EDGE_CURVE('',#4236,#4234,#460,.T.);
#5430=EDGE_CURVE('',#4237,#4235,#461,.T.);
#5431=EDGE_CURVE('',#4238,#4239,#2579,.T.);
#5432=EDGE_CURVE('',#4238,#4236,#462,.T.);
#5433=EDGE_CURVE('',#4239,#4237,#463,.T.);
#5434=EDGE_CURVE('',#4240,#4241,#2580,.T.);
#5435=EDGE_CURVE('',#4240,#4238,#464,.T.);
#5436=EDGE_CURVE('',#4241,#4239,#465,.T.);
#5437=EDGE_CURVE('',#4242,#4243,#2581,.T.);
#5438=EDGE_CURVE('',#4242,#4240,#466,.T.);
#5439=EDGE_CURVE('',#4243,#4241,#467,.T.);
#5440=EDGE_CURVE('',#4244,#4245,#2582,.T.);
#5441=EDGE_CURVE('',#4244,#4242,#468,.T.);
#5442=EDGE_CURVE('',#4245,#4243,#469,.T.);
#5443=EDGE_CURVE('',#4246,#4247,#2583,.T.);
#5444=EDGE_CURVE('',#4246,#4244,#470,.T.);
#5445=EDGE_CURVE('',#4247,#4245,#471,.T.);
#5446=EDGE_CURVE('',#4248,#4249,#2584,.T.);
#5447=EDGE_CURVE('',#4248,#4246,#472,.T.);
#5448=EDGE_CURVE('',#4249,#4247,#473,.T.);
#5449=EDGE_CURVE('',#4250,#4251,#2585,.T.);
#5450=EDGE_CURVE('',#4250,#4248,#474,.T.);
#5451=EDGE_CURVE('',#4251,#4249,#475,.T.);
#5452=EDGE_CURVE('',#4252,#4253,#2586,.T.);
#5453=EDGE_CURVE('',#4252,#4250,#476,.T.);
#5454=EDGE_CURVE('',#4253,#4251,#477,.T.);
#5455=EDGE_CURVE('',#4254,#4255,#2587,.T.);
#5456=EDGE_CURVE('',#4254,#4252,#478,.T.);
#5457=EDGE_CURVE('',#4255,#4253,#479,.T.);
#5458=EDGE_CURVE('',#4256,#4257,#2588,.T.);
#5459=EDGE_CURVE('',#4256,#4254,#480,.T.);
#5460=EDGE_CURVE('',#4257,#4255,#481,.T.);
#5461=EDGE_CURVE('',#4258,#4259,#2589,.T.);
#5462=EDGE_CURVE('',#4258,#4256,#482,.T.);
#5463=EDGE_CURVE('',#4259,#4257,#483,.T.);
#5464=EDGE_CURVE('',#4260,#4261,#2590,.T.);
#5465=EDGE_CURVE('',#4260,#4258,#484,.T.);
#5466=EDGE_CURVE('',#4261,#4259,#485,.T.);
#5467=EDGE_CURVE('',#4262,#4263,#2591,.T.);
#5468=EDGE_CURVE('',#4262,#4260,#486,.T.);
#5469=EDGE_CURVE('',#4263,#4261,#487,.T.);
#5470=EDGE_CURVE('',#4264,#4265,#2592,.T.);
#5471=EDGE_CURVE('',#4264,#4262,#488,.T.);
#5472=EDGE_CURVE('',#4265,#4263,#489,.T.);
#5473=EDGE_CURVE('',#4266,#4267,#2593,.T.);
#5474=EDGE_CURVE('',#4266,#4264,#490,.T.);
#5475=EDGE_CURVE('',#4267,#4265,#491,.T.);
#5476=EDGE_CURVE('',#4209,#4268,#492,.T.);
#5477=EDGE_CURVE('',#4269,#4208,#493,.T.);
#5478=EDGE_CURVE('',#4270,#4269,#3506,.T.);
#5479=EDGE_CURVE('',#4268,#4270,#494,.T.);
#5480=EDGE_CURVE('',#4268,#4271,#2594,.T.);
#5481=EDGE_CURVE('',#4271,#4271,#3507,.T.);
#5482=EDGE_CURVE('',#4272,#4266,#495,.T.);
#5483=EDGE_CURVE('',#4146,#4272,#496,.T.);
#5484=EDGE_CURVE('',#4269,#4204,#497,.T.);
#5485=EDGE_CURVE('',#4273,#4267,#498,.T.);
#5486=EDGE_CURVE('',#4272,#4273,#3508,.T.);
#5487=EDGE_CURVE('',#4205,#4270,#499,.T.);
#5488=EDGE_CURVE('',#4273,#4147,#500,.T.);
#5489=EDGE_CURVE('',#4274,#4275,#2595,.T.);
#5490=EDGE_CURVE('',#4274,#4276,#2596,.T.);
#5491=EDGE_CURVE('',#4276,#4277,#2597,.T.);
#5492=EDGE_CURVE('',#4275,#4277,#2598,.T.);
#5493=EDGE_CURVE('',#4278,#4274,#2599,.T.);
#5494=EDGE_CURVE('',#4278,#4279,#2600,.T.);
#5495=EDGE_CURVE('',#4279,#4276,#2601,.T.);
#5496=EDGE_CURVE('',#4280,#4278,#2602,.T.);
#5497=EDGE_CURVE('',#4280,#4281,#2603,.T.);
#5498=EDGE_CURVE('',#4281,#4279,#2604,.T.);
#5499=EDGE_CURVE('',#4282,#4280,#2605,.T.);
#5500=EDGE_CURVE('',#4282,#4283,#2606,.T.);
#5501=EDGE_CURVE('',#4283,#4281,#2607,.T.);
#5502=EDGE_CURVE('',#4284,#4282,#2608,.T.);
#5503=EDGE_CURVE('',#4284,#4285,#2609,.T.);
#5504=EDGE_CURVE('',#4285,#4283,#2610,.T.);
#5505=EDGE_CURVE('',#4275,#4284,#2611,.T.);
#5506=EDGE_CURVE('',#4277,#4285,#2612,.T.);
#5507=EDGE_CURVE('',#4286,#4286,#3509,.T.);
#5508=EDGE_CURVE('',#4286,#4287,#2613,.T.);
#5509=EDGE_CURVE('',#4287,#4287,#3510,.T.);
#5510=EDGE_CURVE('',#4288,#4289,#2614,.T.);
#5511=EDGE_CURVE('',#4290,#4289,#3511,.F.);
#5512=EDGE_CURVE('',#4290,#4288,#501,.T.);
#5513=EDGE_CURVE('',#4291,#4292,#2615,.T.);
#5514=EDGE_CURVE('',#4292,#4293,#502,.T.);
#5515=EDGE_CURVE('',#4289,#4293,#3512,.F.);
#5516=EDGE_CURVE('',#4288,#4291,#503,.T.);
#5517=EDGE_CURVE('',#4294,#4295,#2616,.T.);
#5518=EDGE_CURVE('',#4295,#4292,#504,.T.);
#5519=EDGE_CURVE('',#4291,#4294,#505,.T.);
#5520=EDGE_CURVE('',#4296,#4297,#2617,.T.);
#5521=EDGE_CURVE('',#4297,#4295,#506,.T.);
#5522=EDGE_CURVE('',#4294,#4296,#507,.T.);
#5523=EDGE_CURVE('',#4298,#4299,#2618,.T.);
#5524=EDGE_CURVE('',#4298,#4300,#508,.T.);
#5525=EDGE_CURVE('',#4301,#4300,#3513,.T.);
#5526=EDGE_CURVE('',#4301,#4299,#509,.T.);
#5527=EDGE_CURVE('',#4302,#4303,#2619,.T.);
#5528=EDGE_CURVE('',#4303,#4304,#510,.T.);
#5529=EDGE_CURVE('',#4305,#4304,#3514,.T.);
#5530=EDGE_CURVE('',#4302,#4305,#511,.T.);
#5531=EDGE_CURVE('',#4306,#4307,#2620,.T.);
#5532=EDGE_CURVE('',#4307,#4303,#512,.T.);
#5533=EDGE_CURVE('',#4306,#4302,#513,.T.);
#5534=EDGE_CURVE('',#4308,#4309,#2621,.T.);
#5535=EDGE_CURVE('',#4309,#4307,#514,.T.);
#5536=EDGE_CURVE('',#4308,#4306,#515,.T.);
#5537=EDGE_CURVE('',#4310,#4311,#2622,.T.);
#5538=EDGE_CURVE('',#4311,#4309,#516,.T.);
#5539=EDGE_CURVE('',#4310,#4308,#517,.T.);
#5540=EDGE_CURVE('',#4312,#4313,#2623,.T.);
#5541=EDGE_CURVE('',#4314,#4312,#518,.T.);
#5542=EDGE_CURVE('',#4315,#4314,#3515,.T.);
#5543=EDGE_CURVE('',#4315,#4313,#519,.T.);
#5544=EDGE_CURVE('',#4313,#4311,#520,.T.);
#5545=EDGE_CURVE('',#4312,#4310,#521,.T.);
#5546=EDGE_CURVE('',#4304,#4290,#522,.T.);
#5547=EDGE_CURVE('',#4300,#4315,#523,.T.);
#5548=EDGE_CURVE('',#4296,#4298,#524,.T.);
#5549=EDGE_CURVE('',#4293,#4305,#525,.T.);
#5550=EDGE_CURVE('',#4299,#4297,#526,.T.);
#5551=EDGE_CURVE('',#4314,#4301,#527,.T.);
#5552=EDGE_CURVE('',#4316,#4317,#2624,.T.);
#5553=EDGE_CURVE('',#4317,#4318,#2625,.T.);
#5554=EDGE_CURVE('',#4318,#4319,#2626,.T.);
#5555=EDGE_CURVE('',#4319,#4320,#2627,.T.);
#5556=EDGE_CURVE('',#4320,#4321,#2628,.T.);
#5557=EDGE_CURVE('',#4321,#4316,#2629,.T.);
#5558=EDGE_CURVE('',#4322,#4323,#2630,.T.);
#5559=EDGE_CURVE('',#4323,#4316,#2631,.T.);
#5560=EDGE_CURVE('',#4322,#4321,#2632,.T.);
#5561=EDGE_CURVE('',#4324,#4322,#2633,.T.);
#5562=EDGE_CURVE('',#4324,#4320,#2634,.T.);
#5563=EDGE_CURVE('',#4325,#4324,#2635,.T.);
#5564=EDGE_CURVE('',#4325,#4319,#2636,.T.);
#5565=EDGE_CURVE('',#4326,#4325,#2637,.T.);
#5566=EDGE_CURVE('',#4326,#4318,#2638,.T.);
#5567=EDGE_CURVE('',#4327,#4326,#2639,.T.);
#5568=EDGE_CURVE('',#4327,#4317,#2640,.T.);
#5569=EDGE_CURVE('',#4323,#4327,#2641,.T.);
#5570=EDGE_CURVE('',#4328,#4328,#3516,.T.);
#5571=EDGE_CURVE('',#4328,#4329,#2642,.T.);
#5572=EDGE_CURVE('',#4329,#4329,#3517,.T.);
#5573=EDGE_CURVE('',#4330,#4330,#3518,.T.);
#5574=EDGE_CURVE('',#4330,#4331,#2643,.T.);
#5575=EDGE_CURVE('',#4331,#4331,#3519,.T.);
#5576=EDGE_CURVE('',#4332,#4332,#3520,.T.);
#5577=EDGE_CURVE('',#4333,#4333,#3521,.T.);
#5578=EDGE_CURVE('',#4334,#4334,#3522,.T.);
#5579=EDGE_CURVE('',#4334,#4332,#2644,.T.);
#5580=EDGE_CURVE('',#4335,#4335,#3523,.T.);
#5581=EDGE_CURVE('',#4336,#4336,#3524,.T.);
#5582=EDGE_CURVE('',#4337,#4337,#3525,.T.);
#5583=EDGE_CURVE('',#4337,#4335,#2645,.T.);
#5584=EDGE_CURVE('',#4338,#4338,#3526,.T.);
#5585=EDGE_CURVE('',#4339,#4339,#3527,.T.);
#5586=EDGE_CURVE('',#4340,#4340,#3528,.T.);
#5587=EDGE_CURVE('',#4340,#4338,#2646,.T.);
#5588=EDGE_CURVE('',#4341,#4341,#3529,.T.);
#5589=EDGE_CURVE('',#4342,#4342,#3530,.T.);
#5590=EDGE_CURVE('',#4343,#4343,#3531,.T.);
#5591=EDGE_CURVE('',#4343,#4341,#2647,.T.);
#5592=EDGE_CURVE('',#4333,#4344,#2648,.T.);
#5593=EDGE_CURVE('',#4344,#4344,#3532,.T.);
#5594=EDGE_CURVE('',#4336,#4345,#2649,.T.);
#5595=EDGE_CURVE('',#4345,#4345,#3533,.T.);
#5596=EDGE_CURVE('',#4339,#4346,#2650,.T.);
#5597=EDGE_CURVE('',#4346,#4346,#3534,.T.);
#5598=EDGE_CURVE('',#4342,#4347,#2651,.T.);
#5599=EDGE_CURVE('',#4347,#4347,#3535,.T.);
#5600=EDGE_CURVE('',#4348,#4349,#3536,.T.);
#5601=EDGE_CURVE('',#4349,#4350,#528,.T.);
#5602=EDGE_CURVE('',#4350,#4351,#3537,.T.);
#5603=EDGE_CURVE('',#4351,#4348,#529,.T.);
#5604=EDGE_CURVE('',#4352,#4353,#3538,.T.);
#5605=EDGE_CURVE('',#4353,#4349,#2652,.T.);
#5606=EDGE_CURVE('',#4348,#4352,#2653,.T.);
#5607=EDGE_CURVE('',#4354,#4355,#3539,.T.);
#5608=EDGE_CURVE('',#4355,#4353,#530,.T.);
#5609=EDGE_CURVE('',#4352,#4354,#531,.T.);
#5610=EDGE_CURVE('',#4356,#4357,#3540,.T.);
#5611=EDGE_CURVE('',#4357,#4355,#532,.T.);
#5612=EDGE_CURVE('',#4354,#4356,#533,.T.);
#5613=EDGE_CURVE('',#4358,#4359,#3541,.T.);
#5614=EDGE_CURVE('',#4359,#4357,#534,.T.);
#5615=EDGE_CURVE('',#4356,#4358,#535,.T.);
#5616=EDGE_CURVE('',#4360,#4361,#3542,.T.);
#5617=EDGE_CURVE('',#4361,#4359,#2654,.T.);
#5618=EDGE_CURVE('',#4358,#4360,#2655,.T.);
#5619=EDGE_CURVE('',#4362,#4363,#3543,.T.);
#5620=EDGE_CURVE('',#4363,#4361,#536,.T.);
#5621=EDGE_CURVE('',#4360,#4362,#537,.T.);
#5622=EDGE_CURVE('',#4350,#4363,#538,.T.);
#5623=EDGE_CURVE('',#4362,#4351,#539,.T.);
#5624=EDGE_CURVE('',#4364,#4361,#540,.T.);
#5625=EDGE_CURVE('',#4365,#4364,#2656,.T.);
#5626=EDGE_CURVE('',#4359,#4365,#541,.T.);
#5627=EDGE_CURVE('',#4363,#4366,#542,.T.);
#5628=EDGE_CURVE('',#4366,#4364,#543,.T.);
#5629=EDGE_CURVE('',#4367,#4350,#544,.T.);
#5630=EDGE_CURVE('',#4366,#4367,#545,.T.);
#5631=EDGE_CURVE('',#4349,#4368,#546,.T.);
#5632=EDGE_CURVE('',#4368,#4367,#547,.T.);
#5633=EDGE_CURVE('',#4369,#4353,#548,.T.);
#5634=EDGE_CURVE('',#4368,#4369,#2657,.T.);
#5635=EDGE_CURVE('',#4365,#4370,#549,.T.);
#5636=EDGE_CURVE('',#4370,#4357,#550,.T.);
#5637=EDGE_CURVE('',#4355,#4371,#551,.T.);
#5638=EDGE_CURVE('',#4371,#4369,#552,.T.);
#5639=EDGE_CURVE('',#4371,#4370,#553,.T.);
#5640=EDGE_CURVE('',#4372,#4372,#3544,.T.);
#5641=EDGE_CURVE('',#4372,#4373,#2658,.T.);
#5642=EDGE_CURVE('',#4373,#4373,#3545,.T.);
#5643=EDGE_CURVE('',#4374,#4374,#3546,.T.);
#5644=EDGE_CURVE('',#4374,#4375,#2659,.T.);
#5645=EDGE_CURVE('',#4375,#4375,#3547,.T.);
#5646=ORIENTED_EDGE('',*,*,#4376,.F.);
#5647=ORIENTED_EDGE('',*,*,#4377,.T.);
#5648=ORIENTED_EDGE('',*,*,#4378,.F.);
#5649=ORIENTED_EDGE('',*,*,#4377,.F.);
#5650=ORIENTED_EDGE('',*,*,#4379,.F.);
#5651=ORIENTED_EDGE('',*,*,#4380,.T.);
#5652=ORIENTED_EDGE('',*,*,#4381,.F.);
#5653=ORIENTED_EDGE('',*,*,#4380,.F.);
#5654=ORIENTED_EDGE('',*,*,#4382,.F.);
#5655=ORIENTED_EDGE('',*,*,#4383,.T.);
#5656=ORIENTED_EDGE('',*,*,#4384,.F.);
#5657=ORIENTED_EDGE('',*,*,#4383,.F.);
#5658=ORIENTED_EDGE('',*,*,#4385,.F.);
#5659=ORIENTED_EDGE('',*,*,#4386,.F.);
#5660=ORIENTED_EDGE('',*,*,#4387,.T.);
#5661=ORIENTED_EDGE('',*,*,#4388,.F.);
#5662=ORIENTED_EDGE('',*,*,#4389,.F.);
#5663=ORIENTED_EDGE('',*,*,#4390,.F.);
#5664=ORIENTED_EDGE('',*,*,#4387,.F.);
#5665=ORIENTED_EDGE('',*,*,#4391,.F.);
#5666=ORIENTED_EDGE('',*,*,#4392,.F.);
#5667=ORIENTED_EDGE('',*,*,#4393,.F.);
#5668=ORIENTED_EDGE('',*,*,#4394,.T.);
#5669=ORIENTED_EDGE('',*,*,#4395,.F.);
#5670=ORIENTED_EDGE('',*,*,#4396,.F.);
#5671=ORIENTED_EDGE('',*,*,#4397,.F.);
#5672=ORIENTED_EDGE('',*,*,#4394,.F.);
#5673=ORIENTED_EDGE('',*,*,#4398,.F.);
#5674=ORIENTED_EDGE('',*,*,#4399,.F.);
#5675=ORIENTED_EDGE('',*,*,#4400,.F.);
#5676=ORIENTED_EDGE('',*,*,#4401,.T.);
#5677=ORIENTED_EDGE('',*,*,#4402,.F.);
#5678=ORIENTED_EDGE('',*,*,#4403,.F.);
#5679=ORIENTED_EDGE('',*,*,#4404,.F.);
#5680=ORIENTED_EDGE('',*,*,#4401,.F.);
#5681=ORIENTED_EDGE('',*,*,#4405,.F.);
#5682=ORIENTED_EDGE('',*,*,#4406,.F.);
#5683=ORIENTED_EDGE('',*,*,#4407,.F.);
#5684=ORIENTED_EDGE('',*,*,#4408,.T.);
#5685=ORIENTED_EDGE('',*,*,#4409,.F.);
#5686=ORIENTED_EDGE('',*,*,#4410,.F.);
#5687=ORIENTED_EDGE('',*,*,#4411,.F.);
#5688=ORIENTED_EDGE('',*,*,#4408,.F.);
#5689=ORIENTED_EDGE('',*,*,#4412,.F.);
#5690=ORIENTED_EDGE('',*,*,#4413,.F.);
#5691=ORIENTED_EDGE('',*,*,#4414,.F.);
#5692=ORIENTED_EDGE('',*,*,#4415,.T.);
#5693=ORIENTED_EDGE('',*,*,#4416,.F.);
#5694=ORIENTED_EDGE('',*,*,#4417,.F.);
#5695=ORIENTED_EDGE('',*,*,#4418,.F.);
#5696=ORIENTED_EDGE('',*,*,#4415,.F.);
#5697=ORIENTED_EDGE('',*,*,#4419,.F.);
#5698=ORIENTED_EDGE('',*,*,#4420,.F.);
#5699=ORIENTED_EDGE('',*,*,#4421,.F.);
#5700=ORIENTED_EDGE('',*,*,#4422,.T.);
#5701=ORIENTED_EDGE('',*,*,#4423,.F.);
#5702=ORIENTED_EDGE('',*,*,#4424,.F.);
#5703=ORIENTED_EDGE('',*,*,#4425,.F.);
#5704=ORIENTED_EDGE('',*,*,#4422,.F.);
#5705=ORIENTED_EDGE('',*,*,#4426,.F.);
#5706=ORIENTED_EDGE('',*,*,#4427,.F.);
#5707=ORIENTED_EDGE('',*,*,#4428,.F.);
#5708=ORIENTED_EDGE('',*,*,#4429,.T.);
#5709=ORIENTED_EDGE('',*,*,#4430,.F.);
#5710=ORIENTED_EDGE('',*,*,#4431,.F.);
#5711=ORIENTED_EDGE('',*,*,#4432,.F.);
#5712=ORIENTED_EDGE('',*,*,#4429,.F.);
#5713=ORIENTED_EDGE('',*,*,#4433,.F.);
#5714=ORIENTED_EDGE('',*,*,#4434,.F.);
#5715=ORIENTED_EDGE('',*,*,#4435,.F.);
#5716=ORIENTED_EDGE('',*,*,#4436,.T.);
#5717=ORIENTED_EDGE('',*,*,#4437,.F.);
#5718=ORIENTED_EDGE('',*,*,#4438,.F.);
#5719=ORIENTED_EDGE('',*,*,#4439,.F.);
#5720=ORIENTED_EDGE('',*,*,#4436,.F.);
#5721=ORIENTED_EDGE('',*,*,#4440,.F.);
#5722=ORIENTED_EDGE('',*,*,#4441,.F.);
#5723=ORIENTED_EDGE('',*,*,#4442,.F.);
#5724=ORIENTED_EDGE('',*,*,#4443,.T.);
#5725=ORIENTED_EDGE('',*,*,#4444,.F.);
#5726=ORIENTED_EDGE('',*,*,#4445,.F.);
#5727=ORIENTED_EDGE('',*,*,#4446,.F.);
#5728=ORIENTED_EDGE('',*,*,#4443,.F.);
#5729=ORIENTED_EDGE('',*,*,#4447,.F.);
#5730=ORIENTED_EDGE('',*,*,#4448,.F.);
#5731=ORIENTED_EDGE('',*,*,#4449,.F.);
#5732=ORIENTED_EDGE('',*,*,#4450,.T.);
#5733=ORIENTED_EDGE('',*,*,#4451,.F.);
#5734=ORIENTED_EDGE('',*,*,#4452,.F.);
#5735=ORIENTED_EDGE('',*,*,#4453,.F.);
#5736=ORIENTED_EDGE('',*,*,#4450,.F.);
#5737=ORIENTED_EDGE('',*,*,#4454,.F.);
#5738=ORIENTED_EDGE('',*,*,#4455,.F.);
#5739=ORIENTED_EDGE('',*,*,#4456,.F.);
#5740=ORIENTED_EDGE('',*,*,#4457,.T.);
#5741=ORIENTED_EDGE('',*,*,#4458,.F.);
#5742=ORIENTED_EDGE('',*,*,#4459,.F.);
#5743=ORIENTED_EDGE('',*,*,#4460,.F.);
#5744=ORIENTED_EDGE('',*,*,#4457,.F.);
#5745=ORIENTED_EDGE('',*,*,#4461,.F.);
#5746=ORIENTED_EDGE('',*,*,#4462,.F.);
#5747=ORIENTED_EDGE('',*,*,#4463,.F.);
#5748=ORIENTED_EDGE('',*,*,#4464,.T.);
#5749=ORIENTED_EDGE('',*,*,#4465,.F.);
#5750=ORIENTED_EDGE('',*,*,#4466,.F.);
#5751=ORIENTED_EDGE('',*,*,#4467,.F.);
#5752=ORIENTED_EDGE('',*,*,#4464,.F.);
#5753=ORIENTED_EDGE('',*,*,#4468,.F.);
#5754=ORIENTED_EDGE('',*,*,#4469,.F.);
#5755=ORIENTED_EDGE('',*,*,#4470,.F.);
#5756=ORIENTED_EDGE('',*,*,#4471,.T.);
#5757=ORIENTED_EDGE('',*,*,#4472,.F.);
#5758=ORIENTED_EDGE('',*,*,#4473,.F.);
#5759=ORIENTED_EDGE('',*,*,#4474,.F.);
#5760=ORIENTED_EDGE('',*,*,#4471,.F.);
#5761=ORIENTED_EDGE('',*,*,#4475,.F.);
#5762=ORIENTED_EDGE('',*,*,#4476,.F.);
#5763=ORIENTED_EDGE('',*,*,#4477,.F.);
#5764=ORIENTED_EDGE('',*,*,#4478,.T.);
#5765=ORIENTED_EDGE('',*,*,#4479,.F.);
#5766=ORIENTED_EDGE('',*,*,#4480,.F.);
#5767=ORIENTED_EDGE('',*,*,#4481,.F.);
#5768=ORIENTED_EDGE('',*,*,#4478,.F.);
#5769=ORIENTED_EDGE('',*,*,#4482,.F.);
#5770=ORIENTED_EDGE('',*,*,#4483,.F.);
#5771=ORIENTED_EDGE('',*,*,#4484,.F.);
#5772=ORIENTED_EDGE('',*,*,#4485,.T.);
#5773=ORIENTED_EDGE('',*,*,#4486,.F.);
#5774=ORIENTED_EDGE('',*,*,#4487,.F.);
#5775=ORIENTED_EDGE('',*,*,#4488,.F.);
#5776=ORIENTED_EDGE('',*,*,#4485,.F.);
#5777=ORIENTED_EDGE('',*,*,#4489,.F.);
#5778=ORIENTED_EDGE('',*,*,#4490,.F.);
#5779=ORIENTED_EDGE('',*,*,#4491,.F.);
#5780=ORIENTED_EDGE('',*,*,#4492,.T.);
#5781=ORIENTED_EDGE('',*,*,#4493,.F.);
#5782=ORIENTED_EDGE('',*,*,#4494,.F.);
#5783=ORIENTED_EDGE('',*,*,#4495,.F.);
#5784=ORIENTED_EDGE('',*,*,#4492,.F.);
#5785=ORIENTED_EDGE('',*,*,#4496,.F.);
#5786=ORIENTED_EDGE('',*,*,#4497,.F.);
#5787=ORIENTED_EDGE('',*,*,#4498,.F.);
#5788=ORIENTED_EDGE('',*,*,#4499,.T.);
#5789=ORIENTED_EDGE('',*,*,#4500,.F.);
#5790=ORIENTED_EDGE('',*,*,#4501,.F.);
#5791=ORIENTED_EDGE('',*,*,#4502,.F.);
#5792=ORIENTED_EDGE('',*,*,#4499,.F.);
#5793=ORIENTED_EDGE('',*,*,#4503,.F.);
#5794=ORIENTED_EDGE('',*,*,#4504,.F.);
#5795=ORIENTED_EDGE('',*,*,#4505,.F.);
#5796=ORIENTED_EDGE('',*,*,#4506,.T.);
#5797=ORIENTED_EDGE('',*,*,#4507,.F.);
#5798=ORIENTED_EDGE('',*,*,#4508,.F.);
#5799=ORIENTED_EDGE('',*,*,#4509,.F.);
#5800=ORIENTED_EDGE('',*,*,#4506,.F.);
#5801=ORIENTED_EDGE('',*,*,#4510,.F.);
#5802=ORIENTED_EDGE('',*,*,#4511,.F.);
#5803=ORIENTED_EDGE('',*,*,#4512,.F.);
#5804=ORIENTED_EDGE('',*,*,#4513,.T.);
#5805=ORIENTED_EDGE('',*,*,#4514,.F.);
#5806=ORIENTED_EDGE('',*,*,#4515,.F.);
#5807=ORIENTED_EDGE('',*,*,#4516,.F.);
#5808=ORIENTED_EDGE('',*,*,#4513,.F.);
#5809=ORIENTED_EDGE('',*,*,#4517,.F.);
#5810=ORIENTED_EDGE('',*,*,#4518,.F.);
#5811=ORIENTED_EDGE('',*,*,#4519,.F.);
#5812=ORIENTED_EDGE('',*,*,#4520,.T.);
#5813=ORIENTED_EDGE('',*,*,#4521,.F.);
#5814=ORIENTED_EDGE('',*,*,#4522,.F.);
#5815=ORIENTED_EDGE('',*,*,#4523,.F.);
#5816=ORIENTED_EDGE('',*,*,#4520,.F.);
#5817=ORIENTED_EDGE('',*,*,#4524,.F.);
#5818=ORIENTED_EDGE('',*,*,#4525,.F.);
#5819=ORIENTED_EDGE('',*,*,#4526,.F.);
#5820=ORIENTED_EDGE('',*,*,#4527,.T.);
#5821=ORIENTED_EDGE('',*,*,#4528,.F.);
#5822=ORIENTED_EDGE('',*,*,#4529,.F.);
#5823=ORIENTED_EDGE('',*,*,#4530,.F.);
#5824=ORIENTED_EDGE('',*,*,#4527,.F.);
#5825=ORIENTED_EDGE('',*,*,#4531,.F.);
#5826=ORIENTED_EDGE('',*,*,#4532,.F.);
#5827=ORIENTED_EDGE('',*,*,#4533,.F.);
#5828=ORIENTED_EDGE('',*,*,#4534,.T.);
#5829=ORIENTED_EDGE('',*,*,#4535,.F.);
#5830=ORIENTED_EDGE('',*,*,#4536,.F.);
#5831=ORIENTED_EDGE('',*,*,#4537,.F.);
#5832=ORIENTED_EDGE('',*,*,#4534,.F.);
#5833=ORIENTED_EDGE('',*,*,#4538,.F.);
#5834=ORIENTED_EDGE('',*,*,#4539,.F.);
#5835=ORIENTED_EDGE('',*,*,#4540,.F.);
#5836=ORIENTED_EDGE('',*,*,#4541,.T.);
#5837=ORIENTED_EDGE('',*,*,#4542,.F.);
#5838=ORIENTED_EDGE('',*,*,#4543,.F.);
#5839=ORIENTED_EDGE('',*,*,#4544,.F.);
#5840=ORIENTED_EDGE('',*,*,#4541,.F.);
#5841=ORIENTED_EDGE('',*,*,#4545,.F.);
#5842=ORIENTED_EDGE('',*,*,#4546,.F.);
#5843=ORIENTED_EDGE('',*,*,#4547,.F.);
#5844=ORIENTED_EDGE('',*,*,#4548,.T.);
#5845=ORIENTED_EDGE('',*,*,#4549,.F.);
#5846=ORIENTED_EDGE('',*,*,#4550,.F.);
#5847=ORIENTED_EDGE('',*,*,#4551,.F.);
#5848=ORIENTED_EDGE('',*,*,#4548,.F.);
#5849=ORIENTED_EDGE('',*,*,#4552,.F.);
#5850=ORIENTED_EDGE('',*,*,#4553,.F.);
#5851=ORIENTED_EDGE('',*,*,#4554,.F.);
#5852=ORIENTED_EDGE('',*,*,#4555,.T.);
#5853=ORIENTED_EDGE('',*,*,#4556,.F.);
#5854=ORIENTED_EDGE('',*,*,#4557,.F.);
#5855=ORIENTED_EDGE('',*,*,#4558,.F.);
#5856=ORIENTED_EDGE('',*,*,#4555,.F.);
#5857=ORIENTED_EDGE('',*,*,#4559,.F.);
#5858=ORIENTED_EDGE('',*,*,#4560,.F.);
#5859=ORIENTED_EDGE('',*,*,#4561,.F.);
#5860=ORIENTED_EDGE('',*,*,#4562,.T.);
#5861=ORIENTED_EDGE('',*,*,#4563,.F.);
#5862=ORIENTED_EDGE('',*,*,#4564,.F.);
#5863=ORIENTED_EDGE('',*,*,#4565,.F.);
#5864=ORIENTED_EDGE('',*,*,#4562,.F.);
#5865=ORIENTED_EDGE('',*,*,#4566,.F.);
#5866=ORIENTED_EDGE('',*,*,#4567,.F.);
#5867=ORIENTED_EDGE('',*,*,#4568,.F.);
#5868=ORIENTED_EDGE('',*,*,#4569,.T.);
#5869=ORIENTED_EDGE('',*,*,#4570,.F.);
#5870=ORIENTED_EDGE('',*,*,#4571,.F.);
#5871=ORIENTED_EDGE('',*,*,#4572,.F.);
#5872=ORIENTED_EDGE('',*,*,#4569,.F.);
#5873=ORIENTED_EDGE('',*,*,#4573,.F.);
#5874=ORIENTED_EDGE('',*,*,#4574,.F.);
#5875=ORIENTED_EDGE('',*,*,#4575,.F.);
#5876=ORIENTED_EDGE('',*,*,#4576,.T.);
#5877=ORIENTED_EDGE('',*,*,#4577,.F.);
#5878=ORIENTED_EDGE('',*,*,#4578,.F.);
#5879=ORIENTED_EDGE('',*,*,#4579,.F.);
#5880=ORIENTED_EDGE('',*,*,#4576,.F.);
#5881=ORIENTED_EDGE('',*,*,#4580,.F.);
#5882=ORIENTED_EDGE('',*,*,#4581,.F.);
#5883=ORIENTED_EDGE('',*,*,#4582,.F.);
#5884=ORIENTED_EDGE('',*,*,#4583,.T.);
#5885=ORIENTED_EDGE('',*,*,#4584,.F.);
#5886=ORIENTED_EDGE('',*,*,#4585,.F.);
#5887=ORIENTED_EDGE('',*,*,#4586,.F.);
#5888=ORIENTED_EDGE('',*,*,#4583,.F.);
#5889=ORIENTED_EDGE('',*,*,#4587,.F.);
#5890=ORIENTED_EDGE('',*,*,#4588,.F.);
#5891=ORIENTED_EDGE('',*,*,#4589,.F.);
#5892=ORIENTED_EDGE('',*,*,#4590,.T.);
#5893=ORIENTED_EDGE('',*,*,#4591,.F.);
#5894=ORIENTED_EDGE('',*,*,#4592,.F.);
#5895=ORIENTED_EDGE('',*,*,#4593,.F.);
#5896=ORIENTED_EDGE('',*,*,#4590,.F.);
#5897=ORIENTED_EDGE('',*,*,#4594,.F.);
#5898=ORIENTED_EDGE('',*,*,#4595,.F.);
#5899=ORIENTED_EDGE('',*,*,#4596,.F.);
#5900=ORIENTED_EDGE('',*,*,#4597,.T.);
#5901=ORIENTED_EDGE('',*,*,#4598,.F.);
#5902=ORIENTED_EDGE('',*,*,#4599,.F.);
#5903=ORIENTED_EDGE('',*,*,#4600,.F.);
#5904=ORIENTED_EDGE('',*,*,#4597,.F.);
#5905=ORIENTED_EDGE('',*,*,#4601,.F.);
#5906=ORIENTED_EDGE('',*,*,#4602,.F.);
#5907=ORIENTED_EDGE('',*,*,#4603,.F.);
#5908=ORIENTED_EDGE('',*,*,#4604,.T.);
#5909=ORIENTED_EDGE('',*,*,#4605,.F.);
#5910=ORIENTED_EDGE('',*,*,#4606,.F.);
#5911=ORIENTED_EDGE('',*,*,#4607,.F.);
#5912=ORIENTED_EDGE('',*,*,#4604,.F.);
#5913=ORIENTED_EDGE('',*,*,#4608,.F.);
#5914=ORIENTED_EDGE('',*,*,#4609,.F.);
#5915=ORIENTED_EDGE('',*,*,#4610,.F.);
#5916=ORIENTED_EDGE('',*,*,#4611,.T.);
#5917=ORIENTED_EDGE('',*,*,#4612,.F.);
#5918=ORIENTED_EDGE('',*,*,#4613,.F.);
#5919=ORIENTED_EDGE('',*,*,#4614,.F.);
#5920=ORIENTED_EDGE('',*,*,#4611,.F.);
#5921=ORIENTED_EDGE('',*,*,#4615,.F.);
#5922=ORIENTED_EDGE('',*,*,#4616,.F.);
#5923=ORIENTED_EDGE('',*,*,#4617,.F.);
#5924=ORIENTED_EDGE('',*,*,#4618,.T.);
#5925=ORIENTED_EDGE('',*,*,#4619,.F.);
#5926=ORIENTED_EDGE('',*,*,#4620,.F.);
#5927=ORIENTED_EDGE('',*,*,#4621,.F.);
#5928=ORIENTED_EDGE('',*,*,#4618,.F.);
#5929=ORIENTED_EDGE('',*,*,#4622,.F.);
#5930=ORIENTED_EDGE('',*,*,#4623,.F.);
#5931=ORIENTED_EDGE('',*,*,#4624,.F.);
#5932=ORIENTED_EDGE('',*,*,#4625,.T.);
#5933=ORIENTED_EDGE('',*,*,#4626,.F.);
#5934=ORIENTED_EDGE('',*,*,#4627,.F.);
#5935=ORIENTED_EDGE('',*,*,#4628,.F.);
#5936=ORIENTED_EDGE('',*,*,#4625,.F.);
#5937=ORIENTED_EDGE('',*,*,#4629,.F.);
#5938=ORIENTED_EDGE('',*,*,#4630,.F.);
#5939=ORIENTED_EDGE('',*,*,#4631,.F.);
#5940=ORIENTED_EDGE('',*,*,#4632,.T.);
#5941=ORIENTED_EDGE('',*,*,#4633,.F.);
#5942=ORIENTED_EDGE('',*,*,#4634,.F.);
#5943=ORIENTED_EDGE('',*,*,#4635,.F.);
#5944=ORIENTED_EDGE('',*,*,#4632,.F.);
#5945=ORIENTED_EDGE('',*,*,#4636,.F.);
#5946=ORIENTED_EDGE('',*,*,#4637,.F.);
#5947=ORIENTED_EDGE('',*,*,#4638,.F.);
#5948=ORIENTED_EDGE('',*,*,#4639,.T.);
#5949=ORIENTED_EDGE('',*,*,#4640,.F.);
#5950=ORIENTED_EDGE('',*,*,#4641,.F.);
#5951=ORIENTED_EDGE('',*,*,#4642,.F.);
#5952=ORIENTED_EDGE('',*,*,#4639,.F.);
#5953=ORIENTED_EDGE('',*,*,#4643,.F.);
#5954=ORIENTED_EDGE('',*,*,#4644,.F.);
#5955=ORIENTED_EDGE('',*,*,#4645,.F.);
#5956=ORIENTED_EDGE('',*,*,#4646,.T.);
#5957=ORIENTED_EDGE('',*,*,#4647,.F.);
#5958=ORIENTED_EDGE('',*,*,#4648,.F.);
#5959=ORIENTED_EDGE('',*,*,#4649,.F.);
#5960=ORIENTED_EDGE('',*,*,#4646,.F.);
#5961=ORIENTED_EDGE('',*,*,#4650,.F.);
#5962=ORIENTED_EDGE('',*,*,#4644,.T.);
#5963=ORIENTED_EDGE('',*,*,#4651,.F.);
#5964=ORIENTED_EDGE('',*,*,#4652,.T.);
#5965=ORIENTED_EDGE('',*,*,#4653,.F.);
#5966=ORIENTED_EDGE('',*,*,#4654,.F.);
#5967=ORIENTED_EDGE('',*,*,#4655,.F.);
#5968=ORIENTED_EDGE('',*,*,#4385,.T.);
#5969=ORIENTED_EDGE('',*,*,#4656,.F.);
#5970=ORIENTED_EDGE('',*,*,#4648,.T.);
#5971=ORIENTED_EDGE('',*,*,#4657,.F.);
#5972=ORIENTED_EDGE('',*,*,#4392,.T.);
#5973=ORIENTED_EDGE('',*,*,#4658,.F.);
#5974=ORIENTED_EDGE('',*,*,#4641,.T.);
#5975=ORIENTED_EDGE('',*,*,#4659,.F.);
#5976=ORIENTED_EDGE('',*,*,#4399,.T.);
#5977=ORIENTED_EDGE('',*,*,#4660,.F.);
#5978=ORIENTED_EDGE('',*,*,#4634,.T.);
#5979=ORIENTED_EDGE('',*,*,#4661,.F.);
#5980=ORIENTED_EDGE('',*,*,#4406,.T.);
#5981=ORIENTED_EDGE('',*,*,#4662,.F.);
#5982=ORIENTED_EDGE('',*,*,#4627,.T.);
#5983=ORIENTED_EDGE('',*,*,#4663,.F.);
#5984=ORIENTED_EDGE('',*,*,#4413,.T.);
#5985=ORIENTED_EDGE('',*,*,#4664,.F.);
#5986=ORIENTED_EDGE('',*,*,#4620,.T.);
#5987=ORIENTED_EDGE('',*,*,#4665,.F.);
#5988=ORIENTED_EDGE('',*,*,#4420,.T.);
#5989=ORIENTED_EDGE('',*,*,#4666,.F.);
#5990=ORIENTED_EDGE('',*,*,#4613,.T.);
#5991=ORIENTED_EDGE('',*,*,#4667,.F.);
#5992=ORIENTED_EDGE('',*,*,#4427,.T.);
#5993=ORIENTED_EDGE('',*,*,#4668,.F.);
#5994=ORIENTED_EDGE('',*,*,#4606,.T.);
#5995=ORIENTED_EDGE('',*,*,#4669,.F.);
#5996=ORIENTED_EDGE('',*,*,#4434,.T.);
#5997=ORIENTED_EDGE('',*,*,#4670,.F.);
#5998=ORIENTED_EDGE('',*,*,#4599,.T.);
#5999=ORIENTED_EDGE('',*,*,#4671,.F.);
#6000=ORIENTED_EDGE('',*,*,#4441,.T.);
#6001=ORIENTED_EDGE('',*,*,#4672,.F.);
#6002=ORIENTED_EDGE('',*,*,#4592,.T.);
#6003=ORIENTED_EDGE('',*,*,#4673,.F.);
#6004=ORIENTED_EDGE('',*,*,#4574,.T.);
#6005=ORIENTED_EDGE('',*,*,#4674,.F.);
#6006=ORIENTED_EDGE('',*,*,#4585,.T.);
#6007=ORIENTED_EDGE('',*,*,#4675,.F.);
#6008=ORIENTED_EDGE('',*,*,#4455,.T.);
#6009=ORIENTED_EDGE('',*,*,#4676,.F.);
#6010=ORIENTED_EDGE('',*,*,#4578,.T.);
#6011=ORIENTED_EDGE('',*,*,#4677,.F.);
#6012=ORIENTED_EDGE('',*,*,#4462,.T.);
#6013=ORIENTED_EDGE('',*,*,#4678,.F.);
#6014=ORIENTED_EDGE('',*,*,#4571,.T.);
#6015=ORIENTED_EDGE('',*,*,#4679,.F.);
#6016=ORIENTED_EDGE('',*,*,#4469,.T.);
#6017=ORIENTED_EDGE('',*,*,#4680,.F.);
#6018=ORIENTED_EDGE('',*,*,#4564,.T.);
#6019=ORIENTED_EDGE('',*,*,#4681,.F.);
#6020=ORIENTED_EDGE('',*,*,#4476,.T.);
#6021=ORIENTED_EDGE('',*,*,#4682,.F.);
#6022=ORIENTED_EDGE('',*,*,#4557,.T.);
#6023=ORIENTED_EDGE('',*,*,#4683,.F.);
#6024=ORIENTED_EDGE('',*,*,#4483,.T.);
#6025=ORIENTED_EDGE('',*,*,#4684,.F.);
#6026=ORIENTED_EDGE('',*,*,#4550,.T.);
#6027=ORIENTED_EDGE('',*,*,#4685,.F.);
#6028=ORIENTED_EDGE('',*,*,#4490,.T.);
#6029=ORIENTED_EDGE('',*,*,#4686,.F.);
#6030=ORIENTED_EDGE('',*,*,#4543,.T.);
#6031=ORIENTED_EDGE('',*,*,#4687,.F.);
#6032=ORIENTED_EDGE('',*,*,#4497,.T.);
#6033=ORIENTED_EDGE('',*,*,#4688,.F.);
#6034=ORIENTED_EDGE('',*,*,#4536,.T.);
#6035=ORIENTED_EDGE('',*,*,#4689,.F.);
#6036=ORIENTED_EDGE('',*,*,#4504,.T.);
#6037=ORIENTED_EDGE('',*,*,#4690,.F.);
#6038=ORIENTED_EDGE('',*,*,#4529,.T.);
#6039=ORIENTED_EDGE('',*,*,#4691,.F.);
#6040=ORIENTED_EDGE('',*,*,#4511,.T.);
#6041=ORIENTED_EDGE('',*,*,#4692,.F.);
#6042=ORIENTED_EDGE('',*,*,#4522,.T.);
#6043=ORIENTED_EDGE('',*,*,#4693,.F.);
#6044=ORIENTED_EDGE('',*,*,#4448,.T.);
#6045=ORIENTED_EDGE('',*,*,#4694,.F.);
#6046=ORIENTED_EDGE('',*,*,#4515,.T.);
#6047=ORIENTED_EDGE('',*,*,#4695,.F.);
#6048=ORIENTED_EDGE('',*,*,#4508,.T.);
#6049=ORIENTED_EDGE('',*,*,#4696,.F.);
#6050=ORIENTED_EDGE('',*,*,#4518,.T.);
#6051=ORIENTED_EDGE('',*,*,#4697,.F.);
#6052=ORIENTED_EDGE('',*,*,#4501,.T.);
#6053=ORIENTED_EDGE('',*,*,#4698,.F.);
#6054=ORIENTED_EDGE('',*,*,#4525,.T.);
#6055=ORIENTED_EDGE('',*,*,#4699,.F.);
#6056=ORIENTED_EDGE('',*,*,#4494,.T.);
#6057=ORIENTED_EDGE('',*,*,#4700,.F.);
#6058=ORIENTED_EDGE('',*,*,#4532,.T.);
#6059=ORIENTED_EDGE('',*,*,#4701,.F.);
#6060=ORIENTED_EDGE('',*,*,#4487,.T.);
#6061=ORIENTED_EDGE('',*,*,#4702,.F.);
#6062=ORIENTED_EDGE('',*,*,#4539,.T.);
#6063=ORIENTED_EDGE('',*,*,#4703,.F.);
#6064=ORIENTED_EDGE('',*,*,#4480,.T.);
#6065=ORIENTED_EDGE('',*,*,#4704,.F.);
#6066=ORIENTED_EDGE('',*,*,#4546,.T.);
#6067=ORIENTED_EDGE('',*,*,#4705,.F.);
#6068=ORIENTED_EDGE('',*,*,#4473,.T.);
#6069=ORIENTED_EDGE('',*,*,#4706,.F.);
#6070=ORIENTED_EDGE('',*,*,#4553,.T.);
#6071=ORIENTED_EDGE('',*,*,#4707,.F.);
#6072=ORIENTED_EDGE('',*,*,#4466,.T.);
#6073=ORIENTED_EDGE('',*,*,#4708,.F.);
#6074=ORIENTED_EDGE('',*,*,#4560,.T.);
#6075=ORIENTED_EDGE('',*,*,#4709,.F.);
#6076=ORIENTED_EDGE('',*,*,#4459,.T.);
#6077=ORIENTED_EDGE('',*,*,#4710,.F.);
#6078=ORIENTED_EDGE('',*,*,#4567,.T.);
#6079=ORIENTED_EDGE('',*,*,#4711,.F.);
#6080=ORIENTED_EDGE('',*,*,#4452,.T.);
#6081=ORIENTED_EDGE('',*,*,#4712,.F.);
#6082=ORIENTED_EDGE('',*,*,#4713,.F.);
#6083=ORIENTED_EDGE('',*,*,#4714,.F.);
#6084=ORIENTED_EDGE('',*,*,#4445,.T.);
#6085=ORIENTED_EDGE('',*,*,#4715,.F.);
#6086=ORIENTED_EDGE('',*,*,#4581,.T.);
#6087=ORIENTED_EDGE('',*,*,#4716,.F.);
#6088=ORIENTED_EDGE('',*,*,#4438,.T.);
#6089=ORIENTED_EDGE('',*,*,#4717,.F.);
#6090=ORIENTED_EDGE('',*,*,#4588,.T.);
#6091=ORIENTED_EDGE('',*,*,#4718,.F.);
#6092=ORIENTED_EDGE('',*,*,#4431,.T.);
#6093=ORIENTED_EDGE('',*,*,#4719,.F.);
#6094=ORIENTED_EDGE('',*,*,#4595,.T.);
#6095=ORIENTED_EDGE('',*,*,#4720,.F.);
#6096=ORIENTED_EDGE('',*,*,#4424,.T.);
#6097=ORIENTED_EDGE('',*,*,#4721,.F.);
#6098=ORIENTED_EDGE('',*,*,#4602,.T.);
#6099=ORIENTED_EDGE('',*,*,#4722,.F.);
#6100=ORIENTED_EDGE('',*,*,#4417,.T.);
#6101=ORIENTED_EDGE('',*,*,#4723,.F.);
#6102=ORIENTED_EDGE('',*,*,#4609,.T.);
#6103=ORIENTED_EDGE('',*,*,#4724,.F.);
#6104=ORIENTED_EDGE('',*,*,#4410,.T.);
#6105=ORIENTED_EDGE('',*,*,#4725,.F.);
#6106=ORIENTED_EDGE('',*,*,#4616,.T.);
#6107=ORIENTED_EDGE('',*,*,#4726,.F.);
#6108=ORIENTED_EDGE('',*,*,#4403,.T.);
#6109=ORIENTED_EDGE('',*,*,#4727,.F.);
#6110=ORIENTED_EDGE('',*,*,#4623,.T.);
#6111=ORIENTED_EDGE('',*,*,#4728,.F.);
#6112=ORIENTED_EDGE('',*,*,#4396,.T.);
#6113=ORIENTED_EDGE('',*,*,#4729,.F.);
#6114=ORIENTED_EDGE('',*,*,#4630,.T.);
#6115=ORIENTED_EDGE('',*,*,#4730,.F.);
#6116=ORIENTED_EDGE('',*,*,#4389,.T.);
#6117=ORIENTED_EDGE('',*,*,#4731,.F.);
#6118=ORIENTED_EDGE('',*,*,#4637,.T.);
#6119=ORIENTED_EDGE('',*,*,#4732,.F.);
#6120=ORIENTED_EDGE('',*,*,#4388,.T.);
#6121=ORIENTED_EDGE('',*,*,#4390,.T.);
#6122=ORIENTED_EDGE('',*,*,#4732,.T.);
#6123=ORIENTED_EDGE('',*,*,#4640,.T.);
#6124=ORIENTED_EDGE('',*,*,#4642,.T.);
#6125=ORIENTED_EDGE('',*,*,#4658,.T.);
#6126=ORIENTED_EDGE('',*,*,#4395,.T.);
#6127=ORIENTED_EDGE('',*,*,#4397,.T.);
#6128=ORIENTED_EDGE('',*,*,#4730,.T.);
#6129=ORIENTED_EDGE('',*,*,#4633,.T.);
#6130=ORIENTED_EDGE('',*,*,#4635,.T.);
#6131=ORIENTED_EDGE('',*,*,#4660,.T.);
#6132=ORIENTED_EDGE('',*,*,#4402,.T.);
#6133=ORIENTED_EDGE('',*,*,#4404,.T.);
#6134=ORIENTED_EDGE('',*,*,#4728,.T.);
#6135=ORIENTED_EDGE('',*,*,#4626,.T.);
#6136=ORIENTED_EDGE('',*,*,#4628,.T.);
#6137=ORIENTED_EDGE('',*,*,#4662,.T.);
#6138=ORIENTED_EDGE('',*,*,#4409,.T.);
#6139=ORIENTED_EDGE('',*,*,#4411,.T.);
#6140=ORIENTED_EDGE('',*,*,#4726,.T.);
#6141=ORIENTED_EDGE('',*,*,#4619,.T.);
#6142=ORIENTED_EDGE('',*,*,#4621,.T.);
#6143=ORIENTED_EDGE('',*,*,#4664,.T.);
#6144=ORIENTED_EDGE('',*,*,#4416,.T.);
#6145=ORIENTED_EDGE('',*,*,#4418,.T.);
#6146=ORIENTED_EDGE('',*,*,#4724,.T.);
#6147=ORIENTED_EDGE('',*,*,#4612,.T.);
#6148=ORIENTED_EDGE('',*,*,#4614,.T.);
#6149=ORIENTED_EDGE('',*,*,#4666,.T.);
#6150=ORIENTED_EDGE('',*,*,#4423,.T.);
#6151=ORIENTED_EDGE('',*,*,#4425,.T.);
#6152=ORIENTED_EDGE('',*,*,#4722,.T.);
#6153=ORIENTED_EDGE('',*,*,#4605,.T.);
#6154=ORIENTED_EDGE('',*,*,#4607,.T.);
#6155=ORIENTED_EDGE('',*,*,#4668,.T.);
#6156=ORIENTED_EDGE('',*,*,#4430,.T.);
#6157=ORIENTED_EDGE('',*,*,#4432,.T.);
#6158=ORIENTED_EDGE('',*,*,#4720,.T.);
#6159=ORIENTED_EDGE('',*,*,#4598,.T.);
#6160=ORIENTED_EDGE('',*,*,#4600,.T.);
#6161=ORIENTED_EDGE('',*,*,#4670,.T.);
#6162=ORIENTED_EDGE('',*,*,#4437,.T.);
#6163=ORIENTED_EDGE('',*,*,#4439,.T.);
#6164=ORIENTED_EDGE('',*,*,#4718,.T.);
#6165=ORIENTED_EDGE('',*,*,#4591,.T.);
#6166=ORIENTED_EDGE('',*,*,#4593,.T.);
#6167=ORIENTED_EDGE('',*,*,#4672,.T.);
#6168=ORIENTED_EDGE('',*,*,#4444,.T.);
#6169=ORIENTED_EDGE('',*,*,#4446,.T.);
#6170=ORIENTED_EDGE('',*,*,#4716,.T.);
#6171=ORIENTED_EDGE('',*,*,#4584,.T.);
#6172=ORIENTED_EDGE('',*,*,#4586,.T.);
#6173=ORIENTED_EDGE('',*,*,#4674,.T.);
#6174=ORIENTED_EDGE('',*,*,#4577,.T.);
#6175=ORIENTED_EDGE('',*,*,#4579,.T.);
#6176=ORIENTED_EDGE('',*,*,#4676,.T.);
#6177=ORIENTED_EDGE('',*,*,#4458,.T.);
#6178=ORIENTED_EDGE('',*,*,#4460,.T.);
#6179=ORIENTED_EDGE('',*,*,#4711,.T.);
#6180=ORIENTED_EDGE('',*,*,#4570,.T.);
#6181=ORIENTED_EDGE('',*,*,#4572,.T.);
#6182=ORIENTED_EDGE('',*,*,#4678,.T.);
#6183=ORIENTED_EDGE('',*,*,#4465,.T.);
#6184=ORIENTED_EDGE('',*,*,#4467,.T.);
#6185=ORIENTED_EDGE('',*,*,#4709,.T.);
#6186=ORIENTED_EDGE('',*,*,#4563,.T.);
#6187=ORIENTED_EDGE('',*,*,#4565,.T.);
#6188=ORIENTED_EDGE('',*,*,#4680,.T.);
#6189=ORIENTED_EDGE('',*,*,#4472,.T.);
#6190=ORIENTED_EDGE('',*,*,#4474,.T.);
#6191=ORIENTED_EDGE('',*,*,#4707,.T.);
#6192=ORIENTED_EDGE('',*,*,#4556,.T.);
#6193=ORIENTED_EDGE('',*,*,#4558,.T.);
#6194=ORIENTED_EDGE('',*,*,#4682,.T.);
#6195=ORIENTED_EDGE('',*,*,#4479,.T.);
#6196=ORIENTED_EDGE('',*,*,#4481,.T.);
#6197=ORIENTED_EDGE('',*,*,#4705,.T.);
#6198=ORIENTED_EDGE('',*,*,#4549,.T.);
#6199=ORIENTED_EDGE('',*,*,#4551,.T.);
#6200=ORIENTED_EDGE('',*,*,#4684,.T.);
#6201=ORIENTED_EDGE('',*,*,#4486,.T.);
#6202=ORIENTED_EDGE('',*,*,#4488,.T.);
#6203=ORIENTED_EDGE('',*,*,#4703,.T.);
#6204=ORIENTED_EDGE('',*,*,#4542,.T.);
#6205=ORIENTED_EDGE('',*,*,#4544,.T.);
#6206=ORIENTED_EDGE('',*,*,#4686,.T.);
#6207=ORIENTED_EDGE('',*,*,#4493,.T.);
#6208=ORIENTED_EDGE('',*,*,#4495,.T.);
#6209=ORIENTED_EDGE('',*,*,#4701,.T.);
#6210=ORIENTED_EDGE('',*,*,#4535,.T.);
#6211=ORIENTED_EDGE('',*,*,#4537,.T.);
#6212=ORIENTED_EDGE('',*,*,#4688,.T.);
#6213=ORIENTED_EDGE('',*,*,#4500,.T.);
#6214=ORIENTED_EDGE('',*,*,#4502,.T.);
#6215=ORIENTED_EDGE('',*,*,#4699,.T.);
#6216=ORIENTED_EDGE('',*,*,#4528,.T.);
#6217=ORIENTED_EDGE('',*,*,#4530,.T.);
#6218=ORIENTED_EDGE('',*,*,#4690,.T.);
#6219=ORIENTED_EDGE('',*,*,#4507,.T.);
#6220=ORIENTED_EDGE('',*,*,#4509,.T.);
#6221=ORIENTED_EDGE('',*,*,#4697,.T.);
#6222=ORIENTED_EDGE('',*,*,#4521,.T.);
#6223=ORIENTED_EDGE('',*,*,#4523,.T.);
#6224=ORIENTED_EDGE('',*,*,#4692,.T.);
#6225=ORIENTED_EDGE('',*,*,#4514,.T.);
#6226=ORIENTED_EDGE('',*,*,#4516,.T.);
#6227=ORIENTED_EDGE('',*,*,#4694,.T.);
#6228=ORIENTED_EDGE('',*,*,#4451,.T.);
#6229=ORIENTED_EDGE('',*,*,#4453,.T.);
#6230=ORIENTED_EDGE('',*,*,#4714,.T.);
#6231=ORIENTED_EDGE('',*,*,#4733,.T.);
#6232=ORIENTED_EDGE('',*,*,#4734,.T.);
#6233=ORIENTED_EDGE('',*,*,#4735,.T.);
#6234=ORIENTED_EDGE('',*,*,#4736,.T.);
#6235=ORIENTED_EDGE('',*,*,#4651,.T.);
#6236=ORIENTED_EDGE('',*,*,#4647,.T.);
#6237=ORIENTED_EDGE('',*,*,#4649,.T.);
#6238=ORIENTED_EDGE('',*,*,#4656,.T.);
#6239=ORIENTED_EDGE('',*,*,#4736,.F.);
#6240=ORIENTED_EDGE('',*,*,#4737,.T.);
#6241=ORIENTED_EDGE('',*,*,#4738,.F.);
#6242=ORIENTED_EDGE('',*,*,#4652,.F.);
#6243=ORIENTED_EDGE('',*,*,#4739,.F.);
#6244=ORIENTED_EDGE('',*,*,#4740,.F.);
#6245=ORIENTED_EDGE('',*,*,#4741,.T.);
#6246=ORIENTED_EDGE('',*,*,#4742,.F.);
#6247=ORIENTED_EDGE('',*,*,#4713,.T.);
#6248=ORIENTED_EDGE('',*,*,#4743,.F.);
#6249=ORIENTED_EDGE('',*,*,#4744,.F.);
#6250=ORIENTED_EDGE('',*,*,#4733,.F.);
#6251=ORIENTED_EDGE('',*,*,#4744,.T.);
#6252=ORIENTED_EDGE('',*,*,#4745,.F.);
#6253=ORIENTED_EDGE('',*,*,#4746,.F.);
#6254=ORIENTED_EDGE('',*,*,#4734,.F.);
#6255=ORIENTED_EDGE('',*,*,#4746,.T.);
#6256=ORIENTED_EDGE('',*,*,#4747,.F.);
#6257=ORIENTED_EDGE('',*,*,#4741,.F.);
#6258=ORIENTED_EDGE('',*,*,#4748,.F.);
#6259=ORIENTED_EDGE('',*,*,#4737,.F.);
#6260=ORIENTED_EDGE('',*,*,#4735,.F.);
#6261=ORIENTED_EDGE('',*,*,#4738,.T.);
#6262=ORIENTED_EDGE('',*,*,#4748,.T.);
#6263=ORIENTED_EDGE('',*,*,#4740,.T.);
#6264=ORIENTED_EDGE('',*,*,#4749,.F.);
#6265=ORIENTED_EDGE('',*,*,#4750,.F.);
#6266=ORIENTED_EDGE('',*,*,#4751,.F.);
#6267=ORIENTED_EDGE('',*,*,#4752,.F.);
#6268=ORIENTED_EDGE('',*,*,#4753,.F.);
#6269=ORIENTED_EDGE('',*,*,#4754,.F.);
#6270=ORIENTED_EDGE('',*,*,#4755,.F.);
#6271=ORIENTED_EDGE('',*,*,#4756,.F.);
#6272=ORIENTED_EDGE('',*,*,#4653,.T.);
#6273=ORIENTED_EDGE('',*,*,#4378,.T.);
#6274=ORIENTED_EDGE('',*,*,#4381,.T.);
#6275=ORIENTED_EDGE('',*,*,#4384,.T.);
#6276=ORIENTED_EDGE('',*,*,#4739,.T.);
#6277=ORIENTED_EDGE('',*,*,#4757,.F.);
#6278=ORIENTED_EDGE('',*,*,#4758,.T.);
#6279=ORIENTED_EDGE('',*,*,#4749,.T.);
#6280=ORIENTED_EDGE('',*,*,#4759,.F.);
#6281=ORIENTED_EDGE('',*,*,#4755,.T.);
#6282=ORIENTED_EDGE('',*,*,#4760,.T.);
#6283=ORIENTED_EDGE('',*,*,#4761,.F.);
#6284=ORIENTED_EDGE('',*,*,#4758,.F.);
#6285=ORIENTED_EDGE('',*,*,#4762,.F.);
#6286=ORIENTED_EDGE('',*,*,#4763,.F.);
#6287=ORIENTED_EDGE('',*,*,#4750,.T.);
#6288=ORIENTED_EDGE('',*,*,#4751,.T.);
#6289=ORIENTED_EDGE('',*,*,#4763,.T.);
#6290=ORIENTED_EDGE('',*,*,#4764,.F.);
#6291=ORIENTED_EDGE('',*,*,#4765,.F.);
#6292=ORIENTED_EDGE('',*,*,#4752,.T.);
#6293=ORIENTED_EDGE('',*,*,#4765,.T.);
#6294=ORIENTED_EDGE('',*,*,#4766,.F.);
#6295=ORIENTED_EDGE('',*,*,#4767,.F.);
#6296=ORIENTED_EDGE('',*,*,#4753,.T.);
#6297=ORIENTED_EDGE('',*,*,#4767,.T.);
#6298=ORIENTED_EDGE('',*,*,#4768,.F.);
#6299=ORIENTED_EDGE('',*,*,#4769,.F.);
#6300=ORIENTED_EDGE('',*,*,#4754,.T.);
#6301=ORIENTED_EDGE('',*,*,#4769,.T.);
#6302=ORIENTED_EDGE('',*,*,#4770,.F.);
#6303=ORIENTED_EDGE('',*,*,#4760,.F.);
#6304=ORIENTED_EDGE('',*,*,#4386,.T.);
#6305=ORIENTED_EDGE('',*,*,#4657,.T.);
#6306=ORIENTED_EDGE('',*,*,#4650,.T.);
#6307=ORIENTED_EDGE('',*,*,#4645,.T.);
#6308=ORIENTED_EDGE('',*,*,#4655,.T.);
#6309=ORIENTED_EDGE('',*,*,#4771,.T.);
#6310=ORIENTED_EDGE('',*,*,#4761,.T.);
#6311=ORIENTED_EDGE('',*,*,#4770,.T.);
#6312=ORIENTED_EDGE('',*,*,#4768,.T.);
#6313=ORIENTED_EDGE('',*,*,#4766,.T.);
#6314=ORIENTED_EDGE('',*,*,#4764,.T.);
#6315=ORIENTED_EDGE('',*,*,#4762,.T.);
#6316=ORIENTED_EDGE('',*,*,#4757,.T.);
#6317=ORIENTED_EDGE('',*,*,#4742,.T.);
#6318=ORIENTED_EDGE('',*,*,#4747,.T.);
#6319=ORIENTED_EDGE('',*,*,#4745,.T.);
#6320=ORIENTED_EDGE('',*,*,#4743,.T.);
#6321=ORIENTED_EDGE('',*,*,#4712,.T.);
#6322=ORIENTED_EDGE('',*,*,#4454,.T.);
#6323=ORIENTED_EDGE('',*,*,#4449,.T.);
#6324=ORIENTED_EDGE('',*,*,#4695,.T.);
#6325=ORIENTED_EDGE('',*,*,#4517,.T.);
#6326=ORIENTED_EDGE('',*,*,#4512,.T.);
#6327=ORIENTED_EDGE('',*,*,#4693,.T.);
#6328=ORIENTED_EDGE('',*,*,#4524,.T.);
#6329=ORIENTED_EDGE('',*,*,#4519,.T.);
#6330=ORIENTED_EDGE('',*,*,#4696,.T.);
#6331=ORIENTED_EDGE('',*,*,#4510,.T.);
#6332=ORIENTED_EDGE('',*,*,#4505,.T.);
#6333=ORIENTED_EDGE('',*,*,#4691,.T.);
#6334=ORIENTED_EDGE('',*,*,#4531,.T.);
#6335=ORIENTED_EDGE('',*,*,#4526,.T.);
#6336=ORIENTED_EDGE('',*,*,#4698,.T.);
#6337=ORIENTED_EDGE('',*,*,#4503,.T.);
#6338=ORIENTED_EDGE('',*,*,#4498,.T.);
#6339=ORIENTED_EDGE('',*,*,#4689,.T.);
#6340=ORIENTED_EDGE('',*,*,#4538,.T.);
#6341=ORIENTED_EDGE('',*,*,#4533,.T.);
#6342=ORIENTED_EDGE('',*,*,#4700,.T.);
#6343=ORIENTED_EDGE('',*,*,#4496,.T.);
#6344=ORIENTED_EDGE('',*,*,#4491,.T.);
#6345=ORIENTED_EDGE('',*,*,#4687,.T.);
#6346=ORIENTED_EDGE('',*,*,#4545,.T.);
#6347=ORIENTED_EDGE('',*,*,#4540,.T.);
#6348=ORIENTED_EDGE('',*,*,#4702,.T.);
#6349=ORIENTED_EDGE('',*,*,#4489,.T.);
#6350=ORIENTED_EDGE('',*,*,#4484,.T.);
#6351=ORIENTED_EDGE('',*,*,#4685,.T.);
#6352=ORIENTED_EDGE('',*,*,#4552,.T.);
#6353=ORIENTED_EDGE('',*,*,#4547,.T.);
#6354=ORIENTED_EDGE('',*,*,#4704,.T.);
#6355=ORIENTED_EDGE('',*,*,#4482,.T.);
#6356=ORIENTED_EDGE('',*,*,#4477,.T.);
#6357=ORIENTED_EDGE('',*,*,#4683,.T.);
#6358=ORIENTED_EDGE('',*,*,#4559,.T.);
#6359=ORIENTED_EDGE('',*,*,#4554,.T.);
#6360=ORIENTED_EDGE('',*,*,#4706,.T.);
#6361=ORIENTED_EDGE('',*,*,#4475,.T.);
#6362=ORIENTED_EDGE('',*,*,#4470,.T.);
#6363=ORIENTED_EDGE('',*,*,#4681,.T.);
#6364=ORIENTED_EDGE('',*,*,#4566,.T.);
#6365=ORIENTED_EDGE('',*,*,#4561,.T.);
#6366=ORIENTED_EDGE('',*,*,#4708,.T.);
#6367=ORIENTED_EDGE('',*,*,#4468,.T.);
#6368=ORIENTED_EDGE('',*,*,#4463,.T.);
#6369=ORIENTED_EDGE('',*,*,#4679,.T.);
#6370=ORIENTED_EDGE('',*,*,#4573,.T.);
#6371=ORIENTED_EDGE('',*,*,#4568,.T.);
#6372=ORIENTED_EDGE('',*,*,#4710,.T.);
#6373=ORIENTED_EDGE('',*,*,#4461,.T.);
#6374=ORIENTED_EDGE('',*,*,#4456,.T.);
#6375=ORIENTED_EDGE('',*,*,#4677,.T.);
#6376=ORIENTED_EDGE('',*,*,#4580,.T.);
#6377=ORIENTED_EDGE('',*,*,#4575,.T.);
#6378=ORIENTED_EDGE('',*,*,#4675,.T.);
#6379=ORIENTED_EDGE('',*,*,#4587,.T.);
#6380=ORIENTED_EDGE('',*,*,#4582,.T.);
#6381=ORIENTED_EDGE('',*,*,#4715,.T.);
#6382=ORIENTED_EDGE('',*,*,#4447,.T.);
#6383=ORIENTED_EDGE('',*,*,#4442,.T.);
#6384=ORIENTED_EDGE('',*,*,#4673,.T.);
#6385=ORIENTED_EDGE('',*,*,#4594,.T.);
#6386=ORIENTED_EDGE('',*,*,#4589,.T.);
#6387=ORIENTED_EDGE('',*,*,#4717,.T.);
#6388=ORIENTED_EDGE('',*,*,#4440,.T.);
#6389=ORIENTED_EDGE('',*,*,#4435,.T.);
#6390=ORIENTED_EDGE('',*,*,#4671,.T.);
#6391=ORIENTED_EDGE('',*,*,#4601,.T.);
#6392=ORIENTED_EDGE('',*,*,#4596,.T.);
#6393=ORIENTED_EDGE('',*,*,#4719,.T.);
#6394=ORIENTED_EDGE('',*,*,#4433,.T.);
#6395=ORIENTED_EDGE('',*,*,#4428,.T.);
#6396=ORIENTED_EDGE('',*,*,#4669,.T.);
#6397=ORIENTED_EDGE('',*,*,#4608,.T.);
#6398=ORIENTED_EDGE('',*,*,#4603,.T.);
#6399=ORIENTED_EDGE('',*,*,#4721,.T.);
#6400=ORIENTED_EDGE('',*,*,#4426,.T.);
#6401=ORIENTED_EDGE('',*,*,#4421,.T.);
#6402=ORIENTED_EDGE('',*,*,#4667,.T.);
#6403=ORIENTED_EDGE('',*,*,#4615,.T.);
#6404=ORIENTED_EDGE('',*,*,#4610,.T.);
#6405=ORIENTED_EDGE('',*,*,#4723,.T.);
#6406=ORIENTED_EDGE('',*,*,#4419,.T.);
#6407=ORIENTED_EDGE('',*,*,#4414,.T.);
#6408=ORIENTED_EDGE('',*,*,#4665,.T.);
#6409=ORIENTED_EDGE('',*,*,#4622,.T.);
#6410=ORIENTED_EDGE('',*,*,#4617,.T.);
#6411=ORIENTED_EDGE('',*,*,#4725,.T.);
#6412=ORIENTED_EDGE('',*,*,#4412,.T.);
#6413=ORIENTED_EDGE('',*,*,#4407,.T.);
#6414=ORIENTED_EDGE('',*,*,#4663,.T.);
#6415=ORIENTED_EDGE('',*,*,#4629,.T.);
#6416=ORIENTED_EDGE('',*,*,#4624,.T.);
#6417=ORIENTED_EDGE('',*,*,#4727,.T.);
#6418=ORIENTED_EDGE('',*,*,#4405,.T.);
#6419=ORIENTED_EDGE('',*,*,#4400,.T.);
#6420=ORIENTED_EDGE('',*,*,#4661,.T.);
#6421=ORIENTED_EDGE('',*,*,#4636,.T.);
#6422=ORIENTED_EDGE('',*,*,#4631,.T.);
#6423=ORIENTED_EDGE('',*,*,#4729,.T.);
#6424=ORIENTED_EDGE('',*,*,#4398,.T.);
#6425=ORIENTED_EDGE('',*,*,#4393,.T.);
#6426=ORIENTED_EDGE('',*,*,#4659,.T.);
#6427=ORIENTED_EDGE('',*,*,#4643,.T.);
#6428=ORIENTED_EDGE('',*,*,#4638,.T.);
#6429=ORIENTED_EDGE('',*,*,#4731,.T.);
#6430=ORIENTED_EDGE('',*,*,#4391,.T.);
#6431=ORIENTED_EDGE('',*,*,#4376,.T.);
#6432=ORIENTED_EDGE('',*,*,#4379,.T.);
#6433=ORIENTED_EDGE('',*,*,#4382,.T.);
#6434=ORIENTED_EDGE('',*,*,#4654,.T.);
#6435=ORIENTED_EDGE('',*,*,#4756,.T.);
#6436=ORIENTED_EDGE('',*,*,#4759,.T.);
#6437=ORIENTED_EDGE('',*,*,#4771,.F.);
#6438=ORIENTED_EDGE('',*,*,#4772,.T.);
#6439=ORIENTED_EDGE('',*,*,#4773,.T.);
#6440=ORIENTED_EDGE('',*,*,#4774,.F.);
#6441=ORIENTED_EDGE('',*,*,#4773,.F.);
#6442=ORIENTED_EDGE('',*,*,#4775,.F.);
#6443=ORIENTED_EDGE('',*,*,#4772,.F.);
#6444=ORIENTED_EDGE('',*,*,#4776,.F.);
#6445=ORIENTED_EDGE('',*,*,#4774,.T.);
#6446=ORIENTED_EDGE('',*,*,#4777,.F.);
#6447=ORIENTED_EDGE('',*,*,#4778,.T.);
#6448=ORIENTED_EDGE('',*,*,#4776,.T.);
#6449=ORIENTED_EDGE('',*,*,#4778,.F.);
#6450=ORIENTED_EDGE('',*,*,#4779,.T.);
#6451=ORIENTED_EDGE('',*,*,#4780,.F.);
#6452=ORIENTED_EDGE('',*,*,#4779,.F.);
#6453=ORIENTED_EDGE('',*,*,#4781,.T.);
#6454=ORIENTED_EDGE('',*,*,#4782,.T.);
#6455=ORIENTED_EDGE('',*,*,#4781,.F.);
#6456=ORIENTED_EDGE('',*,*,#4782,.F.);
#6457=ORIENTED_EDGE('',*,*,#4775,.T.);
#6458=ORIENTED_EDGE('',*,*,#4783,.T.);
#6459=ORIENTED_EDGE('',*,*,#4780,.T.);
#6460=ORIENTED_EDGE('',*,*,#4783,.F.);
#6461=ORIENTED_EDGE('',*,*,#4777,.T.);
#6462=ORIENTED_EDGE('',*,*,#4784,.F.);
#6463=ORIENTED_EDGE('',*,*,#4785,.F.);
#6464=ORIENTED_EDGE('',*,*,#4786,.F.);
#6465=ORIENTED_EDGE('',*,*,#4787,.F.);
#6466=ORIENTED_EDGE('',*,*,#4788,.F.);
#6467=ORIENTED_EDGE('',*,*,#4789,.F.);
#6468=ORIENTED_EDGE('',*,*,#4790,.F.);
#6469=ORIENTED_EDGE('',*,*,#4791,.F.);
#6470=ORIENTED_EDGE('',*,*,#4791,.T.);
#6471=ORIENTED_EDGE('',*,*,#4792,.F.);
#6472=ORIENTED_EDGE('',*,*,#4785,.T.);
#6473=ORIENTED_EDGE('',*,*,#4793,.F.);
#6474=ORIENTED_EDGE('',*,*,#4788,.T.);
#6475=ORIENTED_EDGE('',*,*,#4793,.T.);
#6476=ORIENTED_EDGE('',*,*,#4784,.T.);
#6477=ORIENTED_EDGE('',*,*,#4794,.F.);
#6478=ORIENTED_EDGE('',*,*,#4790,.T.);
#6479=ORIENTED_EDGE('',*,*,#4795,.F.);
#6480=ORIENTED_EDGE('',*,*,#4786,.T.);
#6481=ORIENTED_EDGE('',*,*,#4792,.T.);
#6482=ORIENTED_EDGE('',*,*,#4789,.T.);
#6483=ORIENTED_EDGE('',*,*,#4794,.T.);
#6484=ORIENTED_EDGE('',*,*,#4787,.T.);
#6485=ORIENTED_EDGE('',*,*,#4795,.T.);
#6486=ORIENTED_EDGE('',*,*,#4796,.F.);
#6487=ORIENTED_EDGE('',*,*,#4797,.T.);
#6488=ORIENTED_EDGE('',*,*,#4798,.F.);
#6489=ORIENTED_EDGE('',*,*,#4799,.T.);
#6490=ORIENTED_EDGE('',*,*,#4800,.F.);
#6491=ORIENTED_EDGE('',*,*,#4801,.T.);
#6492=ORIENTED_EDGE('',*,*,#4802,.F.);
#6493=ORIENTED_EDGE('',*,*,#4803,.T.);
#6494=ORIENTED_EDGE('',*,*,#4798,.T.);
#6495=ORIENTED_EDGE('',*,*,#4804,.F.);
#6496=ORIENTED_EDGE('',*,*,#4805,.T.);
#6497=ORIENTED_EDGE('',*,*,#4806,.F.);
#6498=ORIENTED_EDGE('',*,*,#4807,.T.);
#6499=ORIENTED_EDGE('',*,*,#4808,.F.);
#6500=ORIENTED_EDGE('',*,*,#4802,.T.);
#6501=ORIENTED_EDGE('',*,*,#4809,.F.);
#6502=ORIENTED_EDGE('',*,*,#4810,.T.);
#6503=ORIENTED_EDGE('',*,*,#4811,.F.);
#6504=ORIENTED_EDGE('',*,*,#4812,.T.);
#6505=ORIENTED_EDGE('',*,*,#4813,.F.);
#6506=ORIENTED_EDGE('',*,*,#4814,.T.);
#6507=ORIENTED_EDGE('',*,*,#4815,.T.);
#6508=ORIENTED_EDGE('',*,*,#4809,.T.);
#6509=ORIENTED_EDGE('',*,*,#4803,.F.);
#6510=ORIENTED_EDGE('',*,*,#4813,.T.);
#6511=ORIENTED_EDGE('',*,*,#4816,.T.);
#6512=ORIENTED_EDGE('',*,*,#4817,.T.);
#6513=ORIENTED_EDGE('',*,*,#4797,.F.);
#6514=ORIENTED_EDGE('',*,*,#4818,.T.);
#6515=ORIENTED_EDGE('',*,*,#4819,.T.);
#6516=ORIENTED_EDGE('',*,*,#4820,.T.);
#6517=ORIENTED_EDGE('',*,*,#4821,.F.);
#6518=ORIENTED_EDGE('',*,*,#4822,.T.);
#6519=ORIENTED_EDGE('',*,*,#4818,.F.);
#6520=ORIENTED_EDGE('',*,*,#4822,.F.);
#6521=ORIENTED_EDGE('',*,*,#4823,.F.);
#6522=ORIENTED_EDGE('',*,*,#4824,.T.);
#6523=ORIENTED_EDGE('',*,*,#4825,.F.);
#6524=ORIENTED_EDGE('',*,*,#4824,.F.);
#6525=ORIENTED_EDGE('',*,*,#4826,.F.);
#6526=ORIENTED_EDGE('',*,*,#4827,.T.);
#6527=ORIENTED_EDGE('',*,*,#4828,.F.);
#6528=ORIENTED_EDGE('',*,*,#4827,.F.);
#6529=ORIENTED_EDGE('',*,*,#4829,.F.);
#6530=ORIENTED_EDGE('',*,*,#4830,.T.);
#6531=ORIENTED_EDGE('',*,*,#4819,.F.);
#6532=ORIENTED_EDGE('',*,*,#4830,.F.);
#6533=ORIENTED_EDGE('',*,*,#4831,.F.);
#6534=ORIENTED_EDGE('',*,*,#4832,.T.);
#6535=ORIENTED_EDGE('',*,*,#4833,.T.);
#6536=ORIENTED_EDGE('',*,*,#4832,.F.);
#6537=ORIENTED_EDGE('',*,*,#4833,.F.);
#6538=ORIENTED_EDGE('',*,*,#4834,.F.);
#6539=ORIENTED_EDGE('',*,*,#4835,.F.);
#6540=ORIENTED_EDGE('',*,*,#4836,.T.);
#6541=ORIENTED_EDGE('',*,*,#4837,.T.);
#6542=ORIENTED_EDGE('',*,*,#4836,.F.);
#6543=ORIENTED_EDGE('',*,*,#4837,.F.);
#6544=ORIENTED_EDGE('',*,*,#4838,.F.);
#6545=ORIENTED_EDGE('',*,*,#4834,.T.);
#6546=ORIENTED_EDGE('',*,*,#4839,.T.);
#6547=ORIENTED_EDGE('',*,*,#4840,.F.);
#6548=ORIENTED_EDGE('',*,*,#4839,.F.);
#6549=ORIENTED_EDGE('',*,*,#4838,.T.);
#6550=ORIENTED_EDGE('',*,*,#4841,.T.);
#6551=ORIENTED_EDGE('',*,*,#4842,.F.);
#6552=ORIENTED_EDGE('',*,*,#4841,.F.);
#6553=ORIENTED_EDGE('',*,*,#4843,.F.);
#6554=ORIENTED_EDGE('',*,*,#4844,.F.);
#6555=ORIENTED_EDGE('',*,*,#4845,.F.);
#6556=ORIENTED_EDGE('',*,*,#4846,.T.);
#6557=ORIENTED_EDGE('',*,*,#4847,.F.);
#6558=ORIENTED_EDGE('',*,*,#4848,.T.);
#6559=ORIENTED_EDGE('',*,*,#4849,.F.);
#6560=ORIENTED_EDGE('',*,*,#4850,.F.);
#6561=ORIENTED_EDGE('',*,*,#4851,.F.);
#6562=ORIENTED_EDGE('',*,*,#4852,.T.);
#6563=ORIENTED_EDGE('',*,*,#4853,.F.);
#6564=ORIENTED_EDGE('',*,*,#4854,.F.);
#6565=ORIENTED_EDGE('',*,*,#4855,.F.);
#6566=ORIENTED_EDGE('',*,*,#4856,.T.);
#6567=ORIENTED_EDGE('',*,*,#4857,.F.);
#6568=ORIENTED_EDGE('',*,*,#4858,.F.);
#6569=ORIENTED_EDGE('',*,*,#4859,.F.);
#6570=ORIENTED_EDGE('',*,*,#4860,.T.);
#6571=ORIENTED_EDGE('',*,*,#4861,.F.);
#6572=ORIENTED_EDGE('',*,*,#4862,.F.);
#6573=ORIENTED_EDGE('',*,*,#4863,.F.);
#6574=ORIENTED_EDGE('',*,*,#4864,.F.);
#6575=ORIENTED_EDGE('',*,*,#4865,.F.);
#6576=ORIENTED_EDGE('',*,*,#4866,.T.);
#6577=ORIENTED_EDGE('',*,*,#4867,.F.);
#6578=ORIENTED_EDGE('',*,*,#4868,.F.);
#6579=ORIENTED_EDGE('',*,*,#4869,.F.);
#6580=ORIENTED_EDGE('',*,*,#4870,.T.);
#6581=ORIENTED_EDGE('',*,*,#4871,.F.);
#6582=ORIENTED_EDGE('',*,*,#4840,.T.);
#6583=ORIENTED_EDGE('',*,*,#4872,.F.);
#6584=ORIENTED_EDGE('',*,*,#4842,.T.);
#6585=ORIENTED_EDGE('',*,*,#4873,.F.);
#6586=ORIENTED_EDGE('',*,*,#4846,.F.);
#6587=ORIENTED_EDGE('',*,*,#4874,.F.);
#6588=ORIENTED_EDGE('',*,*,#4860,.F.);
#6589=ORIENTED_EDGE('',*,*,#4875,.F.);
#6590=ORIENTED_EDGE('',*,*,#4866,.F.);
#6591=ORIENTED_EDGE('',*,*,#4876,.F.);
#6592=ORIENTED_EDGE('',*,*,#4848,.F.);
#6593=ORIENTED_EDGE('',*,*,#4877,.F.);
#6594=ORIENTED_EDGE('',*,*,#4870,.F.);
#6595=ORIENTED_EDGE('',*,*,#4878,.F.);
#6596=ORIENTED_EDGE('',*,*,#4852,.F.);
#6597=ORIENTED_EDGE('',*,*,#4879,.F.);
#6598=ORIENTED_EDGE('',*,*,#4880,.F.);
#6599=ORIENTED_EDGE('',*,*,#4881,.F.);
#6600=ORIENTED_EDGE('',*,*,#4856,.F.);
#6601=ORIENTED_EDGE('',*,*,#4882,.F.);
#6602=ORIENTED_EDGE('',*,*,#4883,.F.);
#6603=ORIENTED_EDGE('',*,*,#4884,.F.);
#6604=ORIENTED_EDGE('',*,*,#4880,.T.);
#6605=ORIENTED_EDGE('',*,*,#4885,.T.);
#6606=ORIENTED_EDGE('',*,*,#4886,.F.);
#6607=ORIENTED_EDGE('',*,*,#4887,.F.);
#6608=ORIENTED_EDGE('',*,*,#4816,.F.);
#6609=ORIENTED_EDGE('',*,*,#4812,.F.);
#6610=ORIENTED_EDGE('',*,*,#4888,.F.);
#6611=ORIENTED_EDGE('',*,*,#4857,.T.);
#6612=ORIENTED_EDGE('',*,*,#4881,.T.);
#6613=ORIENTED_EDGE('',*,*,#4884,.T.);
#6614=ORIENTED_EDGE('',*,*,#4889,.T.);
#6615=ORIENTED_EDGE('',*,*,#4890,.F.);
#6616=ORIENTED_EDGE('',*,*,#4810,.F.);
#6617=ORIENTED_EDGE('',*,*,#4815,.F.);
#6618=ORIENTED_EDGE('',*,*,#4891,.F.);
#6619=ORIENTED_EDGE('',*,*,#4892,.F.);
#6620=ORIENTED_EDGE('',*,*,#4893,.T.);
#6621=ORIENTED_EDGE('',*,*,#4853,.T.);
#6622=ORIENTED_EDGE('',*,*,#4878,.T.);
#6623=ORIENTED_EDGE('',*,*,#4869,.T.);
#6624=ORIENTED_EDGE('',*,*,#4894,.T.);
#6625=ORIENTED_EDGE('',*,*,#4895,.F.);
#6626=ORIENTED_EDGE('',*,*,#4896,.F.);
#6627=ORIENTED_EDGE('',*,*,#4897,.F.);
#6628=ORIENTED_EDGE('',*,*,#4898,.F.);
#6629=ORIENTED_EDGE('',*,*,#4899,.F.);
#6630=ORIENTED_EDGE('',*,*,#4900,.T.);
#6631=ORIENTED_EDGE('',*,*,#4849,.T.);
#6632=ORIENTED_EDGE('',*,*,#4876,.T.);
#6633=ORIENTED_EDGE('',*,*,#4865,.T.);
#6634=ORIENTED_EDGE('',*,*,#4901,.T.);
#6635=ORIENTED_EDGE('',*,*,#4902,.F.);
#6636=ORIENTED_EDGE('',*,*,#4805,.F.);
#6637=ORIENTED_EDGE('',*,*,#4903,.F.);
#6638=ORIENTED_EDGE('',*,*,#4904,.F.);
#6639=ORIENTED_EDGE('',*,*,#4905,.F.);
#6640=ORIENTED_EDGE('',*,*,#4906,.T.);
#6641=ORIENTED_EDGE('',*,*,#4843,.T.);
#6642=ORIENTED_EDGE('',*,*,#4873,.T.);
#6643=ORIENTED_EDGE('',*,*,#4859,.T.);
#6644=ORIENTED_EDGE('',*,*,#4907,.F.);
#6645=ORIENTED_EDGE('',*,*,#4908,.T.);
#6646=ORIENTED_EDGE('',*,*,#4909,.T.);
#6647=ORIENTED_EDGE('',*,*,#4910,.T.);
#6648=ORIENTED_EDGE('',*,*,#4911,.F.);
#6649=ORIENTED_EDGE('',*,*,#4858,.T.);
#6650=ORIENTED_EDGE('',*,*,#4893,.F.);
#6651=ORIENTED_EDGE('',*,*,#4912,.T.);
#6652=ORIENTED_EDGE('',*,*,#4885,.F.);
#6653=ORIENTED_EDGE('',*,*,#4913,.T.);
#6654=ORIENTED_EDGE('',*,*,#4889,.F.);
#6655=ORIENTED_EDGE('',*,*,#4883,.T.);
#6656=ORIENTED_EDGE('',*,*,#4914,.F.);
#6657=ORIENTED_EDGE('',*,*,#4915,.T.);
#6658=ORIENTED_EDGE('',*,*,#4894,.F.);
#6659=ORIENTED_EDGE('',*,*,#4868,.T.);
#6660=ORIENTED_EDGE('',*,*,#4916,.F.);
#6661=ORIENTED_EDGE('',*,*,#4917,.T.);
#6662=ORIENTED_EDGE('',*,*,#4901,.F.);
#6663=ORIENTED_EDGE('',*,*,#4864,.T.);
#6664=ORIENTED_EDGE('',*,*,#4918,.F.);
#6665=ORIENTED_EDGE('',*,*,#4919,.T.);
#6666=ORIENTED_EDGE('',*,*,#4920,.T.);
#6667=ORIENTED_EDGE('',*,*,#4907,.T.);
#6668=ORIENTED_EDGE('',*,*,#4862,.T.);
#6669=ORIENTED_EDGE('',*,*,#4921,.T.);
#6670=ORIENTED_EDGE('',*,*,#4922,.F.);
#6671=ORIENTED_EDGE('',*,*,#4923,.T.);
#6672=ORIENTED_EDGE('',*,*,#4924,.F.);
#6673=ORIENTED_EDGE('',*,*,#4925,.T.);
#6674=ORIENTED_EDGE('',*,*,#4926,.F.);
#6675=ORIENTED_EDGE('',*,*,#4927,.T.);
#6676=ORIENTED_EDGE('',*,*,#4928,.F.);
#6677=ORIENTED_EDGE('',*,*,#4929,.T.);
#6678=ORIENTED_EDGE('',*,*,#4844,.T.);
#6679=ORIENTED_EDGE('',*,*,#4911,.T.);
#6680=ORIENTED_EDGE('',*,*,#4930,.T.);
#6681=ORIENTED_EDGE('',*,*,#4931,.T.);
#6682=ORIENTED_EDGE('',*,*,#4932,.F.);
#6683=ORIENTED_EDGE('',*,*,#4850,.T.);
#6684=ORIENTED_EDGE('',*,*,#4906,.F.);
#6685=ORIENTED_EDGE('',*,*,#4933,.T.);
#6686=ORIENTED_EDGE('',*,*,#4934,.F.);
#6687=ORIENTED_EDGE('',*,*,#4854,.T.);
#6688=ORIENTED_EDGE('',*,*,#4900,.F.);
#6689=ORIENTED_EDGE('',*,*,#4935,.T.);
#6690=ORIENTED_EDGE('',*,*,#4936,.F.);
#6691=ORIENTED_EDGE('',*,*,#4937,.T.);
#6692=ORIENTED_EDGE('',*,*,#4938,.T.);
#6693=ORIENTED_EDGE('',*,*,#4939,.T.);
#6694=ORIENTED_EDGE('',*,*,#4940,.T.);
#6695=ORIENTED_EDGE('',*,*,#4941,.T.);
#6696=ORIENTED_EDGE('',*,*,#4942,.F.);
#6697=ORIENTED_EDGE('',*,*,#4820,.F.);
#6698=ORIENTED_EDGE('',*,*,#4943,.T.);
#6699=ORIENTED_EDGE('',*,*,#4872,.T.);
#6700=ORIENTED_EDGE('',*,*,#4943,.F.);
#6701=ORIENTED_EDGE('',*,*,#4944,.F.);
#6702=ORIENTED_EDGE('',*,*,#4945,.T.);
#6703=ORIENTED_EDGE('',*,*,#4871,.T.);
#6704=ORIENTED_EDGE('',*,*,#4945,.F.);
#6705=ORIENTED_EDGE('',*,*,#4946,.F.);
#6706=ORIENTED_EDGE('',*,*,#4942,.T.);
#6707=ORIENTED_EDGE('',*,*,#4947,.F.);
#6708=ORIENTED_EDGE('',*,*,#4948,.F.);
#6709=ORIENTED_EDGE('',*,*,#4949,.F.);
#6710=ORIENTED_EDGE('',*,*,#4950,.F.);
#6711=ORIENTED_EDGE('',*,*,#4886,.T.);
#6712=ORIENTED_EDGE('',*,*,#4912,.F.);
#6713=ORIENTED_EDGE('',*,*,#4892,.T.);
#6714=ORIENTED_EDGE('',*,*,#4951,.T.);
#6715=ORIENTED_EDGE('',*,*,#4946,.T.);
#6716=ORIENTED_EDGE('',*,*,#4952,.T.);
#6717=ORIENTED_EDGE('',*,*,#4953,.T.);
#6718=ORIENTED_EDGE('',*,*,#4937,.F.);
#6719=ORIENTED_EDGE('',*,*,#4796,.T.);
#6720=ORIENTED_EDGE('',*,*,#4817,.F.);
#6721=ORIENTED_EDGE('',*,*,#4887,.T.);
#6722=ORIENTED_EDGE('',*,*,#4951,.F.);
#6723=ORIENTED_EDGE('',*,*,#4891,.T.);
#6724=ORIENTED_EDGE('',*,*,#4814,.F.);
#6725=ORIENTED_EDGE('',*,*,#4950,.T.);
#6726=ORIENTED_EDGE('',*,*,#4954,.F.);
#6727=ORIENTED_EDGE('',*,*,#4955,.F.);
#6728=ORIENTED_EDGE('',*,*,#4952,.F.);
#6729=ORIENTED_EDGE('',*,*,#4949,.T.);
#6730=ORIENTED_EDGE('',*,*,#4956,.T.);
#6731=ORIENTED_EDGE('',*,*,#4957,.T.);
#6732=ORIENTED_EDGE('',*,*,#4954,.T.);
#6733=ORIENTED_EDGE('',*,*,#4888,.T.);
#6734=ORIENTED_EDGE('',*,*,#4811,.T.);
#6735=ORIENTED_EDGE('',*,*,#4890,.T.);
#6736=ORIENTED_EDGE('',*,*,#4913,.F.);
#6737=ORIENTED_EDGE('',*,*,#4947,.T.);
#6738=ORIENTED_EDGE('',*,*,#4941,.F.);
#6739=ORIENTED_EDGE('',*,*,#4958,.T.);
#6740=ORIENTED_EDGE('',*,*,#4959,.T.);
#6741=ORIENTED_EDGE('',*,*,#4855,.T.);
#6742=ORIENTED_EDGE('',*,*,#4936,.T.);
#6743=ORIENTED_EDGE('',*,*,#4960,.F.);
#6744=ORIENTED_EDGE('',*,*,#4961,.F.);
#6745=ORIENTED_EDGE('',*,*,#4962,.F.);
#6746=ORIENTED_EDGE('',*,*,#4963,.F.);
#6747=ORIENTED_EDGE('',*,*,#4964,.F.);
#6748=ORIENTED_EDGE('',*,*,#4914,.T.);
#6749=ORIENTED_EDGE('',*,*,#4882,.T.);
#6750=ORIENTED_EDGE('',*,*,#4879,.T.);
#6751=ORIENTED_EDGE('',*,*,#4960,.T.);
#6752=ORIENTED_EDGE('',*,*,#4935,.F.);
#6753=ORIENTED_EDGE('',*,*,#4899,.T.);
#6754=ORIENTED_EDGE('',*,*,#4965,.T.);
#6755=ORIENTED_EDGE('',*,*,#4961,.T.);
#6756=ORIENTED_EDGE('',*,*,#4965,.F.);
#6757=ORIENTED_EDGE('',*,*,#4898,.T.);
#6758=ORIENTED_EDGE('',*,*,#4966,.F.);
#6759=ORIENTED_EDGE('',*,*,#4962,.T.);
#6760=ORIENTED_EDGE('',*,*,#4966,.T.);
#6761=ORIENTED_EDGE('',*,*,#4897,.T.);
#6762=ORIENTED_EDGE('',*,*,#4967,.T.);
#6763=ORIENTED_EDGE('',*,*,#4963,.T.);
#6764=ORIENTED_EDGE('',*,*,#4967,.F.);
#6765=ORIENTED_EDGE('',*,*,#4896,.T.);
#6766=ORIENTED_EDGE('',*,*,#4968,.F.);
#6767=ORIENTED_EDGE('',*,*,#4964,.T.);
#6768=ORIENTED_EDGE('',*,*,#4968,.T.);
#6769=ORIENTED_EDGE('',*,*,#4895,.T.);
#6770=ORIENTED_EDGE('',*,*,#4915,.F.);
#6771=ORIENTED_EDGE('',*,*,#4851,.T.);
#6772=ORIENTED_EDGE('',*,*,#4934,.T.);
#6773=ORIENTED_EDGE('',*,*,#4969,.F.);
#6774=ORIENTED_EDGE('',*,*,#4970,.F.);
#6775=ORIENTED_EDGE('',*,*,#4971,.F.);
#6776=ORIENTED_EDGE('',*,*,#4807,.F.);
#6777=ORIENTED_EDGE('',*,*,#4972,.F.);
#6778=ORIENTED_EDGE('',*,*,#4916,.T.);
#6779=ORIENTED_EDGE('',*,*,#4867,.T.);
#6780=ORIENTED_EDGE('',*,*,#4877,.T.);
#6781=ORIENTED_EDGE('',*,*,#4969,.T.);
#6782=ORIENTED_EDGE('',*,*,#4933,.F.);
#6783=ORIENTED_EDGE('',*,*,#4905,.T.);
#6784=ORIENTED_EDGE('',*,*,#4973,.T.);
#6785=ORIENTED_EDGE('',*,*,#4800,.T.);
#6786=ORIENTED_EDGE('',*,*,#4974,.F.);
#6787=ORIENTED_EDGE('',*,*,#4970,.T.);
#6788=ORIENTED_EDGE('',*,*,#4973,.F.);
#6789=ORIENTED_EDGE('',*,*,#4904,.T.);
#6790=ORIENTED_EDGE('',*,*,#4975,.F.);
#6791=ORIENTED_EDGE('',*,*,#4808,.T.);
#6792=ORIENTED_EDGE('',*,*,#4971,.T.);
#6793=ORIENTED_EDGE('',*,*,#4974,.T.);
#6794=ORIENTED_EDGE('',*,*,#4801,.F.);
#6795=ORIENTED_EDGE('',*,*,#4975,.T.);
#6796=ORIENTED_EDGE('',*,*,#4903,.T.);
#6797=ORIENTED_EDGE('',*,*,#4804,.T.);
#6798=ORIENTED_EDGE('',*,*,#4799,.F.);
#6799=ORIENTED_EDGE('',*,*,#4828,.T.);
#6800=ORIENTED_EDGE('',*,*,#4825,.T.);
#6801=ORIENTED_EDGE('',*,*,#4944,.T.);
#6802=ORIENTED_EDGE('',*,*,#4972,.T.);
#6803=ORIENTED_EDGE('',*,*,#4806,.T.);
#6804=ORIENTED_EDGE('',*,*,#4902,.T.);
#6805=ORIENTED_EDGE('',*,*,#4917,.F.);
#6806=ORIENTED_EDGE('',*,*,#4847,.T.);
#6807=ORIENTED_EDGE('',*,*,#4932,.T.);
#6808=ORIENTED_EDGE('',*,*,#4976,.F.);
#6809=ORIENTED_EDGE('',*,*,#4977,.F.);
#6810=ORIENTED_EDGE('',*,*,#4978,.F.);
#6811=ORIENTED_EDGE('',*,*,#4979,.F.);
#6812=ORIENTED_EDGE('',*,*,#4980,.F.);
#6813=ORIENTED_EDGE('',*,*,#4918,.T.);
#6814=ORIENTED_EDGE('',*,*,#4863,.T.);
#6815=ORIENTED_EDGE('',*,*,#4875,.T.);
#6816=ORIENTED_EDGE('',*,*,#4976,.T.);
#6817=ORIENTED_EDGE('',*,*,#4931,.F.);
#6818=ORIENTED_EDGE('',*,*,#4981,.T.);
#6819=ORIENTED_EDGE('',*,*,#4982,.T.);
#6820=ORIENTED_EDGE('',*,*,#4977,.T.);
#6821=ORIENTED_EDGE('',*,*,#4982,.F.);
#6822=ORIENTED_EDGE('',*,*,#4983,.F.);
#6823=ORIENTED_EDGE('',*,*,#4984,.F.);
#6824=ORIENTED_EDGE('',*,*,#4978,.T.);
#6825=ORIENTED_EDGE('',*,*,#4984,.T.);
#6826=ORIENTED_EDGE('',*,*,#4985,.T.);
#6827=ORIENTED_EDGE('',*,*,#4986,.T.);
#6828=ORIENTED_EDGE('',*,*,#4980,.T.);
#6829=ORIENTED_EDGE('',*,*,#4987,.T.);
#6830=ORIENTED_EDGE('',*,*,#4988,.T.);
#6831=ORIENTED_EDGE('',*,*,#4919,.F.);
#6832=ORIENTED_EDGE('',*,*,#4979,.T.);
#6833=ORIENTED_EDGE('',*,*,#4986,.F.);
#6834=ORIENTED_EDGE('',*,*,#4989,.F.);
#6835=ORIENTED_EDGE('',*,*,#4987,.F.);
#6836=ORIENTED_EDGE('',*,*,#4990,.T.);
#6837=ORIENTED_EDGE('',*,*,#4991,.T.);
#6838=ORIENTED_EDGE('',*,*,#4989,.T.);
#6839=ORIENTED_EDGE('',*,*,#4992,.T.);
#6840=ORIENTED_EDGE('',*,*,#4993,.T.);
#6841=ORIENTED_EDGE('',*,*,#4994,.T.);
#6842=ORIENTED_EDGE('',*,*,#4983,.T.);
#6843=ORIENTED_EDGE('',*,*,#4995,.T.);
#6844=ORIENTED_EDGE('',*,*,#4996,.T.);
#6845=ORIENTED_EDGE('',*,*,#4990,.F.);
#6846=ORIENTED_EDGE('',*,*,#4985,.F.);
#6847=ORIENTED_EDGE('',*,*,#4996,.F.);
#6848=ORIENTED_EDGE('',*,*,#4909,.F.);
#6849=ORIENTED_EDGE('',*,*,#4930,.F.);
#6850=ORIENTED_EDGE('',*,*,#4910,.F.);
#6851=ORIENTED_EDGE('',*,*,#4995,.F.);
#6852=ORIENTED_EDGE('',*,*,#4981,.F.);
#6853=ORIENTED_EDGE('',*,*,#4997,.T.);
#6854=ORIENTED_EDGE('',*,*,#4955,.T.);
#6855=ORIENTED_EDGE('',*,*,#4998,.T.);
#6856=ORIENTED_EDGE('',*,*,#4998,.F.);
#6857=ORIENTED_EDGE('',*,*,#4957,.F.);
#6858=ORIENTED_EDGE('',*,*,#4994,.F.);
#6859=ORIENTED_EDGE('',*,*,#4999,.F.);
#6860=ORIENTED_EDGE('',*,*,#4938,.F.);
#6861=ORIENTED_EDGE('',*,*,#4953,.F.);
#6862=ORIENTED_EDGE('',*,*,#4997,.F.);
#6863=ORIENTED_EDGE('',*,*,#5000,.F.);
#6864=ORIENTED_EDGE('',*,*,#4940,.F.);
#6865=ORIENTED_EDGE('',*,*,#5001,.F.);
#6866=ORIENTED_EDGE('',*,*,#4993,.F.);
#6867=ORIENTED_EDGE('',*,*,#4958,.F.);
#6868=ORIENTED_EDGE('',*,*,#4948,.T.);
#6869=ORIENTED_EDGE('',*,*,#4959,.F.);
#6870=ORIENTED_EDGE('',*,*,#4992,.F.);
#6871=ORIENTED_EDGE('',*,*,#4956,.F.);
#6872=ORIENTED_EDGE('',*,*,#4920,.F.);
#6873=ORIENTED_EDGE('',*,*,#4988,.F.);
#6874=ORIENTED_EDGE('',*,*,#4991,.F.);
#6875=ORIENTED_EDGE('',*,*,#4908,.F.);
#6876=ORIENTED_EDGE('',*,*,#5000,.T.);
#6877=ORIENTED_EDGE('',*,*,#4999,.T.);
#6878=ORIENTED_EDGE('',*,*,#5001,.T.);
#6879=ORIENTED_EDGE('',*,*,#4939,.F.);
#6880=ORIENTED_EDGE('',*,*,#5002,.F.);
#6881=ORIENTED_EDGE('',*,*,#5003,.F.);
#6882=ORIENTED_EDGE('',*,*,#5004,.F.);
#6883=ORIENTED_EDGE('',*,*,#5005,.F.);
#6884=ORIENTED_EDGE('',*,*,#5006,.F.);
#6885=ORIENTED_EDGE('',*,*,#5007,.F.);
#6886=ORIENTED_EDGE('',*,*,#5008,.F.);
#6887=ORIENTED_EDGE('',*,*,#5009,.F.);
#6888=ORIENTED_EDGE('',*,*,#5010,.F.);
#6889=ORIENTED_EDGE('',*,*,#5002,.T.);
#6890=ORIENTED_EDGE('',*,*,#5011,.T.);
#6891=ORIENTED_EDGE('',*,*,#5009,.T.);
#6892=ORIENTED_EDGE('',*,*,#5012,.T.);
#6893=ORIENTED_EDGE('',*,*,#4928,.T.);
#6894=ORIENTED_EDGE('',*,*,#5013,.T.);
#6895=ORIENTED_EDGE('',*,*,#5010,.T.);
#6896=ORIENTED_EDGE('',*,*,#5014,.T.);
#6897=ORIENTED_EDGE('',*,*,#5015,.F.);
#6898=ORIENTED_EDGE('',*,*,#5016,.F.);
#6899=ORIENTED_EDGE('',*,*,#5017,.F.);
#6900=ORIENTED_EDGE('',*,*,#5016,.T.);
#6901=ORIENTED_EDGE('',*,*,#5018,.T.);
#6902=ORIENTED_EDGE('',*,*,#5006,.T.);
#6903=ORIENTED_EDGE('',*,*,#5019,.T.);
#6904=ORIENTED_EDGE('',*,*,#5008,.T.);
#6905=ORIENTED_EDGE('',*,*,#5020,.T.);
#6906=ORIENTED_EDGE('',*,*,#5017,.T.);
#6907=ORIENTED_EDGE('',*,*,#5021,.T.);
#6908=ORIENTED_EDGE('',*,*,#4926,.T.);
#6909=ORIENTED_EDGE('',*,*,#5022,.T.);
#6910=ORIENTED_EDGE('',*,*,#5015,.T.);
#6911=ORIENTED_EDGE('',*,*,#5023,.T.);
#6912=ORIENTED_EDGE('',*,*,#4924,.T.);
#6913=ORIENTED_EDGE('',*,*,#5024,.T.);
#6914=ORIENTED_EDGE('',*,*,#5007,.T.);
#6915=ORIENTED_EDGE('',*,*,#5025,.T.);
#6916=ORIENTED_EDGE('',*,*,#5005,.T.);
#6917=ORIENTED_EDGE('',*,*,#5026,.T.);
#6918=ORIENTED_EDGE('',*,*,#5003,.T.);
#6919=ORIENTED_EDGE('',*,*,#5027,.T.);
#6920=ORIENTED_EDGE('',*,*,#4922,.T.);
#6921=ORIENTED_EDGE('',*,*,#5028,.T.);
#6922=ORIENTED_EDGE('',*,*,#5004,.T.);
#6923=ORIENTED_EDGE('',*,*,#5029,.T.);
#6924=ORIENTED_EDGE('',*,*,#5023,.F.);
#6925=ORIENTED_EDGE('',*,*,#5020,.F.);
#6926=ORIENTED_EDGE('',*,*,#5013,.F.);
#6927=ORIENTED_EDGE('',*,*,#4927,.F.);
#6928=ORIENTED_EDGE('',*,*,#4845,.T.);
#6929=ORIENTED_EDGE('',*,*,#4929,.F.);
#6930=ORIENTED_EDGE('',*,*,#5014,.F.);
#6931=ORIENTED_EDGE('',*,*,#5011,.F.);
#6932=ORIENTED_EDGE('',*,*,#5028,.F.);
#6933=ORIENTED_EDGE('',*,*,#4921,.F.);
#6934=ORIENTED_EDGE('',*,*,#4861,.T.);
#6935=ORIENTED_EDGE('',*,*,#4874,.T.);
#6936=ORIENTED_EDGE('',*,*,#5019,.F.);
#6937=ORIENTED_EDGE('',*,*,#5027,.F.);
#6938=ORIENTED_EDGE('',*,*,#5012,.F.);
#6939=ORIENTED_EDGE('',*,*,#5021,.F.);
#6940=ORIENTED_EDGE('',*,*,#4835,.T.);
#6941=ORIENTED_EDGE('',*,*,#4831,.T.);
#6942=ORIENTED_EDGE('',*,*,#4829,.T.);
#6943=ORIENTED_EDGE('',*,*,#4826,.T.);
#6944=ORIENTED_EDGE('',*,*,#4823,.T.);
#6945=ORIENTED_EDGE('',*,*,#4821,.T.);
#6946=ORIENTED_EDGE('',*,*,#5024,.F.);
#6947=ORIENTED_EDGE('',*,*,#4923,.F.);
#6948=ORIENTED_EDGE('',*,*,#5029,.F.);
#6949=ORIENTED_EDGE('',*,*,#5026,.F.);
#6950=ORIENTED_EDGE('',*,*,#5022,.F.);
#6951=ORIENTED_EDGE('',*,*,#4925,.F.);
#6952=ORIENTED_EDGE('',*,*,#5025,.F.);
#6953=ORIENTED_EDGE('',*,*,#5018,.F.);
#6954=ORIENTED_EDGE('',*,*,#5030,.F.);
#6955=ORIENTED_EDGE('',*,*,#5031,.T.);
#6956=ORIENTED_EDGE('',*,*,#5032,.F.);
#6957=ORIENTED_EDGE('',*,*,#5033,.T.);
#6958=ORIENTED_EDGE('',*,*,#5034,.F.);
#6959=ORIENTED_EDGE('',*,*,#5035,.T.);
#6960=ORIENTED_EDGE('',*,*,#5036,.F.);
#6961=ORIENTED_EDGE('',*,*,#5037,.T.);
#6962=ORIENTED_EDGE('',*,*,#5032,.T.);
#6963=ORIENTED_EDGE('',*,*,#5038,.F.);
#6964=ORIENTED_EDGE('',*,*,#5039,.T.);
#6965=ORIENTED_EDGE('',*,*,#5040,.F.);
#6966=ORIENTED_EDGE('',*,*,#5041,.T.);
#6967=ORIENTED_EDGE('',*,*,#5042,.F.);
#6968=ORIENTED_EDGE('',*,*,#5036,.T.);
#6969=ORIENTED_EDGE('',*,*,#5043,.F.);
#6970=ORIENTED_EDGE('',*,*,#5044,.T.);
#6971=ORIENTED_EDGE('',*,*,#5045,.F.);
#6972=ORIENTED_EDGE('',*,*,#5046,.T.);
#6973=ORIENTED_EDGE('',*,*,#5047,.F.);
#6974=ORIENTED_EDGE('',*,*,#5048,.T.);
#6975=ORIENTED_EDGE('',*,*,#5049,.T.);
#6976=ORIENTED_EDGE('',*,*,#5043,.T.);
#6977=ORIENTED_EDGE('',*,*,#5037,.F.);
#6978=ORIENTED_EDGE('',*,*,#5047,.T.);
#6979=ORIENTED_EDGE('',*,*,#5050,.T.);
#6980=ORIENTED_EDGE('',*,*,#5051,.T.);
#6981=ORIENTED_EDGE('',*,*,#5031,.F.);
#6982=ORIENTED_EDGE('',*,*,#5052,.T.);
#6983=ORIENTED_EDGE('',*,*,#5053,.T.);
#6984=ORIENTED_EDGE('',*,*,#5054,.T.);
#6985=ORIENTED_EDGE('',*,*,#5055,.F.);
#6986=ORIENTED_EDGE('',*,*,#5056,.T.);
#6987=ORIENTED_EDGE('',*,*,#5057,.T.);
#6988=ORIENTED_EDGE('',*,*,#5058,.F.);
#6989=ORIENTED_EDGE('',*,*,#5059,.F.);
#6990=ORIENTED_EDGE('',*,*,#5060,.T.);
#6991=ORIENTED_EDGE('',*,*,#5061,.T.);
#6992=ORIENTED_EDGE('',*,*,#5056,.F.);
#6993=ORIENTED_EDGE('',*,*,#5062,.F.);
#6994=ORIENTED_EDGE('',*,*,#5063,.T.);
#6995=ORIENTED_EDGE('',*,*,#5064,.T.);
#6996=ORIENTED_EDGE('',*,*,#5060,.F.);
#6997=ORIENTED_EDGE('',*,*,#5065,.F.);
#6998=ORIENTED_EDGE('',*,*,#5066,.T.);
#6999=ORIENTED_EDGE('',*,*,#5067,.T.);
#7000=ORIENTED_EDGE('',*,*,#5063,.F.);
#7001=ORIENTED_EDGE('',*,*,#5068,.F.);
#7002=ORIENTED_EDGE('',*,*,#5069,.T.);
#7003=ORIENTED_EDGE('',*,*,#5070,.T.);
#7004=ORIENTED_EDGE('',*,*,#5066,.F.);
#7005=ORIENTED_EDGE('',*,*,#5071,.F.);
#7006=ORIENTED_EDGE('',*,*,#5058,.T.);
#7007=ORIENTED_EDGE('',*,*,#5072,.T.);
#7008=ORIENTED_EDGE('',*,*,#5069,.F.);
#7009=ORIENTED_EDGE('',*,*,#5072,.F.);
#7010=ORIENTED_EDGE('',*,*,#5057,.F.);
#7011=ORIENTED_EDGE('',*,*,#5061,.F.);
#7012=ORIENTED_EDGE('',*,*,#5064,.F.);
#7013=ORIENTED_EDGE('',*,*,#5067,.F.);
#7014=ORIENTED_EDGE('',*,*,#5070,.F.);
#7015=ORIENTED_EDGE('',*,*,#5073,.F.);
#7016=ORIENTED_EDGE('',*,*,#5074,.F.);
#7017=ORIENTED_EDGE('',*,*,#5075,.T.);
#7018=ORIENTED_EDGE('',*,*,#5076,.T.);
#7019=ORIENTED_EDGE('',*,*,#5077,.F.);
#7020=ORIENTED_EDGE('',*,*,#5078,.F.);
#7021=ORIENTED_EDGE('',*,*,#5079,.T.);
#7022=ORIENTED_EDGE('',*,*,#5080,.T.);
#7023=ORIENTED_EDGE('',*,*,#5075,.F.);
#7024=ORIENTED_EDGE('',*,*,#5081,.F.);
#7025=ORIENTED_EDGE('',*,*,#5082,.T.);
#7026=ORIENTED_EDGE('',*,*,#5083,.T.);
#7027=ORIENTED_EDGE('',*,*,#5079,.F.);
#7028=ORIENTED_EDGE('',*,*,#5084,.F.);
#7029=ORIENTED_EDGE('',*,*,#5085,.T.);
#7030=ORIENTED_EDGE('',*,*,#5086,.T.);
#7031=ORIENTED_EDGE('',*,*,#5082,.F.);
#7032=ORIENTED_EDGE('',*,*,#5087,.F.);
#7033=ORIENTED_EDGE('',*,*,#5088,.T.);
#7034=ORIENTED_EDGE('',*,*,#5089,.T.);
#7035=ORIENTED_EDGE('',*,*,#5085,.F.);
#7036=ORIENTED_EDGE('',*,*,#5090,.F.);
#7037=ORIENTED_EDGE('',*,*,#5077,.T.);
#7038=ORIENTED_EDGE('',*,*,#5091,.T.);
#7039=ORIENTED_EDGE('',*,*,#5088,.F.);
#7040=ORIENTED_EDGE('',*,*,#5091,.F.);
#7041=ORIENTED_EDGE('',*,*,#5076,.F.);
#7042=ORIENTED_EDGE('',*,*,#5080,.F.);
#7043=ORIENTED_EDGE('',*,*,#5083,.F.);
#7044=ORIENTED_EDGE('',*,*,#5086,.F.);
#7045=ORIENTED_EDGE('',*,*,#5089,.F.);
#7046=ORIENTED_EDGE('',*,*,#5092,.F.);
#7047=ORIENTED_EDGE('',*,*,#5093,.F.);
#7048=ORIENTED_EDGE('',*,*,#5094,.T.);
#7049=ORIENTED_EDGE('',*,*,#5052,.F.);
#7050=ORIENTED_EDGE('',*,*,#5094,.F.);
#7051=ORIENTED_EDGE('',*,*,#5095,.F.);
#7052=ORIENTED_EDGE('',*,*,#5096,.T.);
#7053=ORIENTED_EDGE('',*,*,#5097,.F.);
#7054=ORIENTED_EDGE('',*,*,#5096,.F.);
#7055=ORIENTED_EDGE('',*,*,#5098,.F.);
#7056=ORIENTED_EDGE('',*,*,#5099,.T.);
#7057=ORIENTED_EDGE('',*,*,#5100,.F.);
#7058=ORIENTED_EDGE('',*,*,#5099,.F.);
#7059=ORIENTED_EDGE('',*,*,#5101,.F.);
#7060=ORIENTED_EDGE('',*,*,#5102,.T.);
#7061=ORIENTED_EDGE('',*,*,#5053,.F.);
#7062=ORIENTED_EDGE('',*,*,#5102,.F.);
#7063=ORIENTED_EDGE('',*,*,#5092,.T.);
#7064=ORIENTED_EDGE('',*,*,#5103,.T.);
#7065=ORIENTED_EDGE('',*,*,#5104,.F.);
#7066=ORIENTED_EDGE('',*,*,#5103,.F.);
#7067=ORIENTED_EDGE('',*,*,#5073,.T.);
#7068=ORIENTED_EDGE('',*,*,#5105,.T.);
#7069=ORIENTED_EDGE('',*,*,#5106,.F.);
#7070=ORIENTED_EDGE('',*,*,#5105,.F.);
#7071=ORIENTED_EDGE('',*,*,#5107,.F.);
#7072=ORIENTED_EDGE('',*,*,#5108,.F.);
#7073=ORIENTED_EDGE('',*,*,#5109,.F.);
#7074=ORIENTED_EDGE('',*,*,#5110,.T.);
#7075=ORIENTED_EDGE('',*,*,#5111,.F.);
#7076=ORIENTED_EDGE('',*,*,#5112,.T.);
#7077=ORIENTED_EDGE('',*,*,#5113,.F.);
#7078=ORIENTED_EDGE('',*,*,#5114,.F.);
#7079=ORIENTED_EDGE('',*,*,#5115,.F.);
#7080=ORIENTED_EDGE('',*,*,#5116,.T.);
#7081=ORIENTED_EDGE('',*,*,#5117,.F.);
#7082=ORIENTED_EDGE('',*,*,#5118,.F.);
#7083=ORIENTED_EDGE('',*,*,#5119,.F.);
#7084=ORIENTED_EDGE('',*,*,#5120,.T.);
#7085=ORIENTED_EDGE('',*,*,#5121,.F.);
#7086=ORIENTED_EDGE('',*,*,#5122,.F.);
#7087=ORIENTED_EDGE('',*,*,#5123,.F.);
#7088=ORIENTED_EDGE('',*,*,#5124,.T.);
#7089=ORIENTED_EDGE('',*,*,#5125,.F.);
#7090=ORIENTED_EDGE('',*,*,#5126,.F.);
#7091=ORIENTED_EDGE('',*,*,#5127,.F.);
#7092=ORIENTED_EDGE('',*,*,#5128,.F.);
#7093=ORIENTED_EDGE('',*,*,#5129,.F.);
#7094=ORIENTED_EDGE('',*,*,#5130,.T.);
#7095=ORIENTED_EDGE('',*,*,#5131,.F.);
#7096=ORIENTED_EDGE('',*,*,#5132,.F.);
#7097=ORIENTED_EDGE('',*,*,#5133,.F.);
#7098=ORIENTED_EDGE('',*,*,#5134,.T.);
#7099=ORIENTED_EDGE('',*,*,#5135,.F.);
#7100=ORIENTED_EDGE('',*,*,#5104,.T.);
#7101=ORIENTED_EDGE('',*,*,#5136,.F.);
#7102=ORIENTED_EDGE('',*,*,#5106,.T.);
#7103=ORIENTED_EDGE('',*,*,#5137,.F.);
#7104=ORIENTED_EDGE('',*,*,#5110,.F.);
#7105=ORIENTED_EDGE('',*,*,#5138,.F.);
#7106=ORIENTED_EDGE('',*,*,#5124,.F.);
#7107=ORIENTED_EDGE('',*,*,#5139,.F.);
#7108=ORIENTED_EDGE('',*,*,#5130,.F.);
#7109=ORIENTED_EDGE('',*,*,#5140,.F.);
#7110=ORIENTED_EDGE('',*,*,#5112,.F.);
#7111=ORIENTED_EDGE('',*,*,#5141,.F.);
#7112=ORIENTED_EDGE('',*,*,#5134,.F.);
#7113=ORIENTED_EDGE('',*,*,#5142,.F.);
#7114=ORIENTED_EDGE('',*,*,#5116,.F.);
#7115=ORIENTED_EDGE('',*,*,#5143,.F.);
#7116=ORIENTED_EDGE('',*,*,#5144,.F.);
#7117=ORIENTED_EDGE('',*,*,#5145,.F.);
#7118=ORIENTED_EDGE('',*,*,#5120,.F.);
#7119=ORIENTED_EDGE('',*,*,#5146,.F.);
#7120=ORIENTED_EDGE('',*,*,#5147,.F.);
#7121=ORIENTED_EDGE('',*,*,#5148,.F.);
#7122=ORIENTED_EDGE('',*,*,#5144,.T.);
#7123=ORIENTED_EDGE('',*,*,#5149,.T.);
#7124=ORIENTED_EDGE('',*,*,#5150,.F.);
#7125=ORIENTED_EDGE('',*,*,#5151,.F.);
#7126=ORIENTED_EDGE('',*,*,#5050,.F.);
#7127=ORIENTED_EDGE('',*,*,#5046,.F.);
#7128=ORIENTED_EDGE('',*,*,#5152,.F.);
#7129=ORIENTED_EDGE('',*,*,#5121,.T.);
#7130=ORIENTED_EDGE('',*,*,#5145,.T.);
#7131=ORIENTED_EDGE('',*,*,#5148,.T.);
#7132=ORIENTED_EDGE('',*,*,#5153,.T.);
#7133=ORIENTED_EDGE('',*,*,#5154,.F.);
#7134=ORIENTED_EDGE('',*,*,#5044,.F.);
#7135=ORIENTED_EDGE('',*,*,#5049,.F.);
#7136=ORIENTED_EDGE('',*,*,#5155,.F.);
#7137=ORIENTED_EDGE('',*,*,#5156,.F.);
#7138=ORIENTED_EDGE('',*,*,#5157,.T.);
#7139=ORIENTED_EDGE('',*,*,#5117,.T.);
#7140=ORIENTED_EDGE('',*,*,#5142,.T.);
#7141=ORIENTED_EDGE('',*,*,#5133,.T.);
#7142=ORIENTED_EDGE('',*,*,#5158,.T.);
#7143=ORIENTED_EDGE('',*,*,#5159,.F.);
#7144=ORIENTED_EDGE('',*,*,#5160,.F.);
#7145=ORIENTED_EDGE('',*,*,#5161,.F.);
#7146=ORIENTED_EDGE('',*,*,#5162,.F.);
#7147=ORIENTED_EDGE('',*,*,#5163,.F.);
#7148=ORIENTED_EDGE('',*,*,#5164,.T.);
#7149=ORIENTED_EDGE('',*,*,#5113,.T.);
#7150=ORIENTED_EDGE('',*,*,#5140,.T.);
#7151=ORIENTED_EDGE('',*,*,#5129,.T.);
#7152=ORIENTED_EDGE('',*,*,#5165,.T.);
#7153=ORIENTED_EDGE('',*,*,#5166,.F.);
#7154=ORIENTED_EDGE('',*,*,#5039,.F.);
#7155=ORIENTED_EDGE('',*,*,#5167,.F.);
#7156=ORIENTED_EDGE('',*,*,#5168,.F.);
#7157=ORIENTED_EDGE('',*,*,#5169,.F.);
#7158=ORIENTED_EDGE('',*,*,#5170,.T.);
#7159=ORIENTED_EDGE('',*,*,#5107,.T.);
#7160=ORIENTED_EDGE('',*,*,#5137,.T.);
#7161=ORIENTED_EDGE('',*,*,#5123,.T.);
#7162=ORIENTED_EDGE('',*,*,#5171,.F.);
#7163=ORIENTED_EDGE('',*,*,#5172,.T.);
#7164=ORIENTED_EDGE('',*,*,#5173,.T.);
#7165=ORIENTED_EDGE('',*,*,#5174,.T.);
#7166=ORIENTED_EDGE('',*,*,#5175,.F.);
#7167=ORIENTED_EDGE('',*,*,#5122,.T.);
#7168=ORIENTED_EDGE('',*,*,#5157,.F.);
#7169=ORIENTED_EDGE('',*,*,#5176,.T.);
#7170=ORIENTED_EDGE('',*,*,#5149,.F.);
#7171=ORIENTED_EDGE('',*,*,#5177,.T.);
#7172=ORIENTED_EDGE('',*,*,#5153,.F.);
#7173=ORIENTED_EDGE('',*,*,#5147,.T.);
#7174=ORIENTED_EDGE('',*,*,#5178,.F.);
#7175=ORIENTED_EDGE('',*,*,#5179,.T.);
#7176=ORIENTED_EDGE('',*,*,#5158,.F.);
#7177=ORIENTED_EDGE('',*,*,#5132,.T.);
#7178=ORIENTED_EDGE('',*,*,#5180,.F.);
#7179=ORIENTED_EDGE('',*,*,#5181,.T.);
#7180=ORIENTED_EDGE('',*,*,#5165,.F.);
#7181=ORIENTED_EDGE('',*,*,#5128,.T.);
#7182=ORIENTED_EDGE('',*,*,#5182,.F.);
#7183=ORIENTED_EDGE('',*,*,#5183,.T.);
#7184=ORIENTED_EDGE('',*,*,#5184,.T.);
#7185=ORIENTED_EDGE('',*,*,#5171,.T.);
#7186=ORIENTED_EDGE('',*,*,#5126,.T.);
#7187=ORIENTED_EDGE('',*,*,#5185,.T.);
#7188=ORIENTED_EDGE('',*,*,#5186,.F.);
#7189=ORIENTED_EDGE('',*,*,#5187,.T.);
#7190=ORIENTED_EDGE('',*,*,#5188,.F.);
#7191=ORIENTED_EDGE('',*,*,#5189,.T.);
#7192=ORIENTED_EDGE('',*,*,#5190,.F.);
#7193=ORIENTED_EDGE('',*,*,#5191,.T.);
#7194=ORIENTED_EDGE('',*,*,#5192,.F.);
#7195=ORIENTED_EDGE('',*,*,#5193,.T.);
#7196=ORIENTED_EDGE('',*,*,#5108,.T.);
#7197=ORIENTED_EDGE('',*,*,#5175,.T.);
#7198=ORIENTED_EDGE('',*,*,#5194,.T.);
#7199=ORIENTED_EDGE('',*,*,#5195,.T.);
#7200=ORIENTED_EDGE('',*,*,#5196,.F.);
#7201=ORIENTED_EDGE('',*,*,#5114,.T.);
#7202=ORIENTED_EDGE('',*,*,#5170,.F.);
#7203=ORIENTED_EDGE('',*,*,#5197,.T.);
#7204=ORIENTED_EDGE('',*,*,#5198,.F.);
#7205=ORIENTED_EDGE('',*,*,#5118,.T.);
#7206=ORIENTED_EDGE('',*,*,#5164,.F.);
#7207=ORIENTED_EDGE('',*,*,#5199,.T.);
#7208=ORIENTED_EDGE('',*,*,#5200,.F.);
#7209=ORIENTED_EDGE('',*,*,#5201,.T.);
#7210=ORIENTED_EDGE('',*,*,#5202,.T.);
#7211=ORIENTED_EDGE('',*,*,#5203,.T.);
#7212=ORIENTED_EDGE('',*,*,#5204,.T.);
#7213=ORIENTED_EDGE('',*,*,#5205,.T.);
#7214=ORIENTED_EDGE('',*,*,#5206,.F.);
#7215=ORIENTED_EDGE('',*,*,#5054,.F.);
#7216=ORIENTED_EDGE('',*,*,#5207,.T.);
#7217=ORIENTED_EDGE('',*,*,#5136,.T.);
#7218=ORIENTED_EDGE('',*,*,#5207,.F.);
#7219=ORIENTED_EDGE('',*,*,#5208,.F.);
#7220=ORIENTED_EDGE('',*,*,#5209,.T.);
#7221=ORIENTED_EDGE('',*,*,#5135,.T.);
#7222=ORIENTED_EDGE('',*,*,#5209,.F.);
#7223=ORIENTED_EDGE('',*,*,#5210,.F.);
#7224=ORIENTED_EDGE('',*,*,#5206,.T.);
#7225=ORIENTED_EDGE('',*,*,#5211,.F.);
#7226=ORIENTED_EDGE('',*,*,#5212,.F.);
#7227=ORIENTED_EDGE('',*,*,#5213,.F.);
#7228=ORIENTED_EDGE('',*,*,#5214,.F.);
#7229=ORIENTED_EDGE('',*,*,#5150,.T.);
#7230=ORIENTED_EDGE('',*,*,#5176,.F.);
#7231=ORIENTED_EDGE('',*,*,#5156,.T.);
#7232=ORIENTED_EDGE('',*,*,#5215,.T.);
#7233=ORIENTED_EDGE('',*,*,#5210,.T.);
#7234=ORIENTED_EDGE('',*,*,#5216,.T.);
#7235=ORIENTED_EDGE('',*,*,#5217,.T.);
#7236=ORIENTED_EDGE('',*,*,#5201,.F.);
#7237=ORIENTED_EDGE('',*,*,#5030,.T.);
#7238=ORIENTED_EDGE('',*,*,#5051,.F.);
#7239=ORIENTED_EDGE('',*,*,#5151,.T.);
#7240=ORIENTED_EDGE('',*,*,#5215,.F.);
#7241=ORIENTED_EDGE('',*,*,#5155,.T.);
#7242=ORIENTED_EDGE('',*,*,#5048,.F.);
#7243=ORIENTED_EDGE('',*,*,#5214,.T.);
#7244=ORIENTED_EDGE('',*,*,#5218,.F.);
#7245=ORIENTED_EDGE('',*,*,#5219,.F.);
#7246=ORIENTED_EDGE('',*,*,#5216,.F.);
#7247=ORIENTED_EDGE('',*,*,#5213,.T.);
#7248=ORIENTED_EDGE('',*,*,#5220,.T.);
#7249=ORIENTED_EDGE('',*,*,#5221,.T.);
#7250=ORIENTED_EDGE('',*,*,#5218,.T.);
#7251=ORIENTED_EDGE('',*,*,#5152,.T.);
#7252=ORIENTED_EDGE('',*,*,#5045,.T.);
#7253=ORIENTED_EDGE('',*,*,#5154,.T.);
#7254=ORIENTED_EDGE('',*,*,#5177,.F.);
#7255=ORIENTED_EDGE('',*,*,#5211,.T.);
#7256=ORIENTED_EDGE('',*,*,#5205,.F.);
#7257=ORIENTED_EDGE('',*,*,#5222,.T.);
#7258=ORIENTED_EDGE('',*,*,#5223,.T.);
#7259=ORIENTED_EDGE('',*,*,#5119,.T.);
#7260=ORIENTED_EDGE('',*,*,#5200,.T.);
#7261=ORIENTED_EDGE('',*,*,#5224,.F.);
#7262=ORIENTED_EDGE('',*,*,#5225,.F.);
#7263=ORIENTED_EDGE('',*,*,#5226,.F.);
#7264=ORIENTED_EDGE('',*,*,#5227,.F.);
#7265=ORIENTED_EDGE('',*,*,#5228,.F.);
#7266=ORIENTED_EDGE('',*,*,#5178,.T.);
#7267=ORIENTED_EDGE('',*,*,#5146,.T.);
#7268=ORIENTED_EDGE('',*,*,#5143,.T.);
#7269=ORIENTED_EDGE('',*,*,#5224,.T.);
#7270=ORIENTED_EDGE('',*,*,#5199,.F.);
#7271=ORIENTED_EDGE('',*,*,#5163,.T.);
#7272=ORIENTED_EDGE('',*,*,#5229,.T.);
#7273=ORIENTED_EDGE('',*,*,#5225,.T.);
#7274=ORIENTED_EDGE('',*,*,#5229,.F.);
#7275=ORIENTED_EDGE('',*,*,#5162,.T.);
#7276=ORIENTED_EDGE('',*,*,#5230,.F.);
#7277=ORIENTED_EDGE('',*,*,#5226,.T.);
#7278=ORIENTED_EDGE('',*,*,#5230,.T.);
#7279=ORIENTED_EDGE('',*,*,#5161,.T.);
#7280=ORIENTED_EDGE('',*,*,#5231,.T.);
#7281=ORIENTED_EDGE('',*,*,#5227,.T.);
#7282=ORIENTED_EDGE('',*,*,#5231,.F.);
#7283=ORIENTED_EDGE('',*,*,#5160,.T.);
#7284=ORIENTED_EDGE('',*,*,#5232,.F.);
#7285=ORIENTED_EDGE('',*,*,#5228,.T.);
#7286=ORIENTED_EDGE('',*,*,#5232,.T.);
#7287=ORIENTED_EDGE('',*,*,#5159,.T.);
#7288=ORIENTED_EDGE('',*,*,#5179,.F.);
#7289=ORIENTED_EDGE('',*,*,#5115,.T.);
#7290=ORIENTED_EDGE('',*,*,#5198,.T.);
#7291=ORIENTED_EDGE('',*,*,#5233,.F.);
#7292=ORIENTED_EDGE('',*,*,#5234,.F.);
#7293=ORIENTED_EDGE('',*,*,#5235,.F.);
#7294=ORIENTED_EDGE('',*,*,#5041,.F.);
#7295=ORIENTED_EDGE('',*,*,#5236,.F.);
#7296=ORIENTED_EDGE('',*,*,#5180,.T.);
#7297=ORIENTED_EDGE('',*,*,#5131,.T.);
#7298=ORIENTED_EDGE('',*,*,#5141,.T.);
#7299=ORIENTED_EDGE('',*,*,#5233,.T.);
#7300=ORIENTED_EDGE('',*,*,#5197,.F.);
#7301=ORIENTED_EDGE('',*,*,#5169,.T.);
#7302=ORIENTED_EDGE('',*,*,#5237,.T.);
#7303=ORIENTED_EDGE('',*,*,#5034,.T.);
#7304=ORIENTED_EDGE('',*,*,#5238,.F.);
#7305=ORIENTED_EDGE('',*,*,#5234,.T.);
#7306=ORIENTED_EDGE('',*,*,#5237,.F.);
#7307=ORIENTED_EDGE('',*,*,#5168,.T.);
#7308=ORIENTED_EDGE('',*,*,#5239,.F.);
#7309=ORIENTED_EDGE('',*,*,#5042,.T.);
#7310=ORIENTED_EDGE('',*,*,#5235,.T.);
#7311=ORIENTED_EDGE('',*,*,#5238,.T.);
#7312=ORIENTED_EDGE('',*,*,#5035,.F.);
#7313=ORIENTED_EDGE('',*,*,#5239,.T.);
#7314=ORIENTED_EDGE('',*,*,#5167,.T.);
#7315=ORIENTED_EDGE('',*,*,#5038,.T.);
#7316=ORIENTED_EDGE('',*,*,#5033,.F.);
#7317=ORIENTED_EDGE('',*,*,#5100,.T.);
#7318=ORIENTED_EDGE('',*,*,#5097,.T.);
#7319=ORIENTED_EDGE('',*,*,#5208,.T.);
#7320=ORIENTED_EDGE('',*,*,#5236,.T.);
#7321=ORIENTED_EDGE('',*,*,#5040,.T.);
#7322=ORIENTED_EDGE('',*,*,#5166,.T.);
#7323=ORIENTED_EDGE('',*,*,#5181,.F.);
#7324=ORIENTED_EDGE('',*,*,#5111,.T.);
#7325=ORIENTED_EDGE('',*,*,#5196,.T.);
#7326=ORIENTED_EDGE('',*,*,#5240,.F.);
#7327=ORIENTED_EDGE('',*,*,#5241,.F.);
#7328=ORIENTED_EDGE('',*,*,#5242,.F.);
#7329=ORIENTED_EDGE('',*,*,#5243,.F.);
#7330=ORIENTED_EDGE('',*,*,#5244,.F.);
#7331=ORIENTED_EDGE('',*,*,#5182,.T.);
#7332=ORIENTED_EDGE('',*,*,#5127,.T.);
#7333=ORIENTED_EDGE('',*,*,#5139,.T.);
#7334=ORIENTED_EDGE('',*,*,#5240,.T.);
#7335=ORIENTED_EDGE('',*,*,#5195,.F.);
#7336=ORIENTED_EDGE('',*,*,#5245,.T.);
#7337=ORIENTED_EDGE('',*,*,#5246,.T.);
#7338=ORIENTED_EDGE('',*,*,#5241,.T.);
#7339=ORIENTED_EDGE('',*,*,#5246,.F.);
#7340=ORIENTED_EDGE('',*,*,#5247,.F.);
#7341=ORIENTED_EDGE('',*,*,#5248,.F.);
#7342=ORIENTED_EDGE('',*,*,#5242,.T.);
#7343=ORIENTED_EDGE('',*,*,#5248,.T.);
#7344=ORIENTED_EDGE('',*,*,#5249,.T.);
#7345=ORIENTED_EDGE('',*,*,#5250,.T.);
#7346=ORIENTED_EDGE('',*,*,#5244,.T.);
#7347=ORIENTED_EDGE('',*,*,#5251,.T.);
#7348=ORIENTED_EDGE('',*,*,#5252,.T.);
#7349=ORIENTED_EDGE('',*,*,#5183,.F.);
#7350=ORIENTED_EDGE('',*,*,#5243,.T.);
#7351=ORIENTED_EDGE('',*,*,#5250,.F.);
#7352=ORIENTED_EDGE('',*,*,#5253,.F.);
#7353=ORIENTED_EDGE('',*,*,#5251,.F.);
#7354=ORIENTED_EDGE('',*,*,#5254,.T.);
#7355=ORIENTED_EDGE('',*,*,#5255,.T.);
#7356=ORIENTED_EDGE('',*,*,#5253,.T.);
#7357=ORIENTED_EDGE('',*,*,#5256,.T.);
#7358=ORIENTED_EDGE('',*,*,#5257,.T.);
#7359=ORIENTED_EDGE('',*,*,#5258,.T.);
#7360=ORIENTED_EDGE('',*,*,#5247,.T.);
#7361=ORIENTED_EDGE('',*,*,#5259,.T.);
#7362=ORIENTED_EDGE('',*,*,#5260,.T.);
#7363=ORIENTED_EDGE('',*,*,#5254,.F.);
#7364=ORIENTED_EDGE('',*,*,#5249,.F.);
#7365=ORIENTED_EDGE('',*,*,#5260,.F.);
#7366=ORIENTED_EDGE('',*,*,#5173,.F.);
#7367=ORIENTED_EDGE('',*,*,#5194,.F.);
#7368=ORIENTED_EDGE('',*,*,#5174,.F.);
#7369=ORIENTED_EDGE('',*,*,#5259,.F.);
#7370=ORIENTED_EDGE('',*,*,#5245,.F.);
#7371=ORIENTED_EDGE('',*,*,#5261,.T.);
#7372=ORIENTED_EDGE('',*,*,#5219,.T.);
#7373=ORIENTED_EDGE('',*,*,#5262,.T.);
#7374=ORIENTED_EDGE('',*,*,#5262,.F.);
#7375=ORIENTED_EDGE('',*,*,#5221,.F.);
#7376=ORIENTED_EDGE('',*,*,#5258,.F.);
#7377=ORIENTED_EDGE('',*,*,#5263,.F.);
#7378=ORIENTED_EDGE('',*,*,#5202,.F.);
#7379=ORIENTED_EDGE('',*,*,#5217,.F.);
#7380=ORIENTED_EDGE('',*,*,#5261,.F.);
#7381=ORIENTED_EDGE('',*,*,#5264,.F.);
#7382=ORIENTED_EDGE('',*,*,#5204,.F.);
#7383=ORIENTED_EDGE('',*,*,#5265,.F.);
#7384=ORIENTED_EDGE('',*,*,#5257,.F.);
#7385=ORIENTED_EDGE('',*,*,#5222,.F.);
#7386=ORIENTED_EDGE('',*,*,#5212,.T.);
#7387=ORIENTED_EDGE('',*,*,#5223,.F.);
#7388=ORIENTED_EDGE('',*,*,#5256,.F.);
#7389=ORIENTED_EDGE('',*,*,#5220,.F.);
#7390=ORIENTED_EDGE('',*,*,#5184,.F.);
#7391=ORIENTED_EDGE('',*,*,#5252,.F.);
#7392=ORIENTED_EDGE('',*,*,#5255,.F.);
#7393=ORIENTED_EDGE('',*,*,#5172,.F.);
#7394=ORIENTED_EDGE('',*,*,#5264,.T.);
#7395=ORIENTED_EDGE('',*,*,#5263,.T.);
#7396=ORIENTED_EDGE('',*,*,#5265,.T.);
#7397=ORIENTED_EDGE('',*,*,#5203,.F.);
#7398=ORIENTED_EDGE('',*,*,#5266,.F.);
#7399=ORIENTED_EDGE('',*,*,#5267,.F.);
#7400=ORIENTED_EDGE('',*,*,#5268,.F.);
#7401=ORIENTED_EDGE('',*,*,#5269,.F.);
#7402=ORIENTED_EDGE('',*,*,#5270,.F.);
#7403=ORIENTED_EDGE('',*,*,#5271,.F.);
#7404=ORIENTED_EDGE('',*,*,#5272,.F.);
#7405=ORIENTED_EDGE('',*,*,#5273,.F.);
#7406=ORIENTED_EDGE('',*,*,#5274,.F.);
#7407=ORIENTED_EDGE('',*,*,#5266,.T.);
#7408=ORIENTED_EDGE('',*,*,#5275,.T.);
#7409=ORIENTED_EDGE('',*,*,#5273,.T.);
#7410=ORIENTED_EDGE('',*,*,#5276,.T.);
#7411=ORIENTED_EDGE('',*,*,#5192,.T.);
#7412=ORIENTED_EDGE('',*,*,#5277,.T.);
#7413=ORIENTED_EDGE('',*,*,#5274,.T.);
#7414=ORIENTED_EDGE('',*,*,#5278,.T.);
#7415=ORIENTED_EDGE('',*,*,#5279,.F.);
#7416=ORIENTED_EDGE('',*,*,#5280,.F.);
#7417=ORIENTED_EDGE('',*,*,#5281,.F.);
#7418=ORIENTED_EDGE('',*,*,#5280,.T.);
#7419=ORIENTED_EDGE('',*,*,#5282,.T.);
#7420=ORIENTED_EDGE('',*,*,#5270,.T.);
#7421=ORIENTED_EDGE('',*,*,#5283,.T.);
#7422=ORIENTED_EDGE('',*,*,#5272,.T.);
#7423=ORIENTED_EDGE('',*,*,#5284,.T.);
#7424=ORIENTED_EDGE('',*,*,#5281,.T.);
#7425=ORIENTED_EDGE('',*,*,#5285,.T.);
#7426=ORIENTED_EDGE('',*,*,#5190,.T.);
#7427=ORIENTED_EDGE('',*,*,#5286,.T.);
#7428=ORIENTED_EDGE('',*,*,#5279,.T.);
#7429=ORIENTED_EDGE('',*,*,#5287,.T.);
#7430=ORIENTED_EDGE('',*,*,#5188,.T.);
#7431=ORIENTED_EDGE('',*,*,#5288,.T.);
#7432=ORIENTED_EDGE('',*,*,#5271,.T.);
#7433=ORIENTED_EDGE('',*,*,#5289,.T.);
#7434=ORIENTED_EDGE('',*,*,#5269,.T.);
#7435=ORIENTED_EDGE('',*,*,#5290,.T.);
#7436=ORIENTED_EDGE('',*,*,#5267,.T.);
#7437=ORIENTED_EDGE('',*,*,#5291,.T.);
#7438=ORIENTED_EDGE('',*,*,#5186,.T.);
#7439=ORIENTED_EDGE('',*,*,#5292,.T.);
#7440=ORIENTED_EDGE('',*,*,#5268,.T.);
#7441=ORIENTED_EDGE('',*,*,#5293,.T.);
#7442=ORIENTED_EDGE('',*,*,#5287,.F.);
#7443=ORIENTED_EDGE('',*,*,#5284,.F.);
#7444=ORIENTED_EDGE('',*,*,#5277,.F.);
#7445=ORIENTED_EDGE('',*,*,#5191,.F.);
#7446=ORIENTED_EDGE('',*,*,#5109,.T.);
#7447=ORIENTED_EDGE('',*,*,#5193,.F.);
#7448=ORIENTED_EDGE('',*,*,#5278,.F.);
#7449=ORIENTED_EDGE('',*,*,#5275,.F.);
#7450=ORIENTED_EDGE('',*,*,#5292,.F.);
#7451=ORIENTED_EDGE('',*,*,#5185,.F.);
#7452=ORIENTED_EDGE('',*,*,#5125,.T.);
#7453=ORIENTED_EDGE('',*,*,#5138,.T.);
#7454=ORIENTED_EDGE('',*,*,#5283,.F.);
#7455=ORIENTED_EDGE('',*,*,#5291,.F.);
#7456=ORIENTED_EDGE('',*,*,#5276,.F.);
#7457=ORIENTED_EDGE('',*,*,#5285,.F.);
#7458=ORIENTED_EDGE('',*,*,#5055,.T.);
#7459=ORIENTED_EDGE('',*,*,#5071,.T.);
#7460=ORIENTED_EDGE('',*,*,#5068,.T.);
#7461=ORIENTED_EDGE('',*,*,#5065,.T.);
#7462=ORIENTED_EDGE('',*,*,#5062,.T.);
#7463=ORIENTED_EDGE('',*,*,#5059,.T.);
#7464=ORIENTED_EDGE('',*,*,#5074,.T.);
#7465=ORIENTED_EDGE('',*,*,#5090,.T.);
#7466=ORIENTED_EDGE('',*,*,#5087,.T.);
#7467=ORIENTED_EDGE('',*,*,#5084,.T.);
#7468=ORIENTED_EDGE('',*,*,#5081,.T.);
#7469=ORIENTED_EDGE('',*,*,#5078,.T.);
#7470=ORIENTED_EDGE('',*,*,#5101,.T.);
#7471=ORIENTED_EDGE('',*,*,#5098,.T.);
#7472=ORIENTED_EDGE('',*,*,#5095,.T.);
#7473=ORIENTED_EDGE('',*,*,#5093,.T.);
#7474=ORIENTED_EDGE('',*,*,#5288,.F.);
#7475=ORIENTED_EDGE('',*,*,#5187,.F.);
#7476=ORIENTED_EDGE('',*,*,#5293,.F.);
#7477=ORIENTED_EDGE('',*,*,#5290,.F.);
#7478=ORIENTED_EDGE('',*,*,#5286,.F.);
#7479=ORIENTED_EDGE('',*,*,#5189,.F.);
#7480=ORIENTED_EDGE('',*,*,#5289,.F.);
#7481=ORIENTED_EDGE('',*,*,#5282,.F.);
#7482=ORIENTED_EDGE('',*,*,#5294,.F.);
#7483=ORIENTED_EDGE('',*,*,#5295,.T.);
#7484=ORIENTED_EDGE('',*,*,#5296,.T.);
#7485=ORIENTED_EDGE('',*,*,#5297,.T.);
#7486=ORIENTED_EDGE('',*,*,#5298,.F.);
#7487=ORIENTED_EDGE('',*,*,#5299,.T.);
#7488=ORIENTED_EDGE('',*,*,#5294,.T.);
#7489=ORIENTED_EDGE('',*,*,#5300,.T.);
#7490=ORIENTED_EDGE('',*,*,#5301,.F.);
#7491=ORIENTED_EDGE('',*,*,#5302,.T.);
#7492=ORIENTED_EDGE('',*,*,#5298,.T.);
#7493=ORIENTED_EDGE('',*,*,#5303,.T.);
#7494=ORIENTED_EDGE('',*,*,#5304,.F.);
#7495=ORIENTED_EDGE('',*,*,#5305,.T.);
#7496=ORIENTED_EDGE('',*,*,#5301,.T.);
#7497=ORIENTED_EDGE('',*,*,#5306,.T.);
#7498=ORIENTED_EDGE('',*,*,#5307,.F.);
#7499=ORIENTED_EDGE('',*,*,#5308,.T.);
#7500=ORIENTED_EDGE('',*,*,#5304,.T.);
#7501=ORIENTED_EDGE('',*,*,#5309,.T.);
#7502=ORIENTED_EDGE('',*,*,#5310,.F.);
#7503=ORIENTED_EDGE('',*,*,#5311,.T.);
#7504=ORIENTED_EDGE('',*,*,#5307,.T.);
#7505=ORIENTED_EDGE('',*,*,#5312,.T.);
#7506=ORIENTED_EDGE('',*,*,#5313,.F.);
#7507=ORIENTED_EDGE('',*,*,#5314,.T.);
#7508=ORIENTED_EDGE('',*,*,#5310,.T.);
#7509=ORIENTED_EDGE('',*,*,#5315,.T.);
#7510=ORIENTED_EDGE('',*,*,#5316,.F.);
#7511=ORIENTED_EDGE('',*,*,#5317,.T.);
#7512=ORIENTED_EDGE('',*,*,#5313,.T.);
#7513=ORIENTED_EDGE('',*,*,#5318,.T.);
#7514=ORIENTED_EDGE('',*,*,#5319,.F.);
#7515=ORIENTED_EDGE('',*,*,#5320,.T.);
#7516=ORIENTED_EDGE('',*,*,#5316,.T.);
#7517=ORIENTED_EDGE('',*,*,#5321,.T.);
#7518=ORIENTED_EDGE('',*,*,#5322,.F.);
#7519=ORIENTED_EDGE('',*,*,#5323,.T.);
#7520=ORIENTED_EDGE('',*,*,#5319,.T.);
#7521=ORIENTED_EDGE('',*,*,#5324,.T.);
#7522=ORIENTED_EDGE('',*,*,#5325,.F.);
#7523=ORIENTED_EDGE('',*,*,#5326,.T.);
#7524=ORIENTED_EDGE('',*,*,#5322,.T.);
#7525=ORIENTED_EDGE('',*,*,#5327,.T.);
#7526=ORIENTED_EDGE('',*,*,#5328,.F.);
#7527=ORIENTED_EDGE('',*,*,#5329,.T.);
#7528=ORIENTED_EDGE('',*,*,#5325,.T.);
#7529=ORIENTED_EDGE('',*,*,#5330,.T.);
#7530=ORIENTED_EDGE('',*,*,#5331,.F.);
#7531=ORIENTED_EDGE('',*,*,#5332,.T.);
#7532=ORIENTED_EDGE('',*,*,#5328,.T.);
#7533=ORIENTED_EDGE('',*,*,#5333,.T.);
#7534=ORIENTED_EDGE('',*,*,#5334,.F.);
#7535=ORIENTED_EDGE('',*,*,#5335,.T.);
#7536=ORIENTED_EDGE('',*,*,#5331,.T.);
#7537=ORIENTED_EDGE('',*,*,#5336,.T.);
#7538=ORIENTED_EDGE('',*,*,#5337,.F.);
#7539=ORIENTED_EDGE('',*,*,#5338,.T.);
#7540=ORIENTED_EDGE('',*,*,#5334,.T.);
#7541=ORIENTED_EDGE('',*,*,#5339,.T.);
#7542=ORIENTED_EDGE('',*,*,#5340,.F.);
#7543=ORIENTED_EDGE('',*,*,#5341,.T.);
#7544=ORIENTED_EDGE('',*,*,#5337,.T.);
#7545=ORIENTED_EDGE('',*,*,#5342,.T.);
#7546=ORIENTED_EDGE('',*,*,#5343,.F.);
#7547=ORIENTED_EDGE('',*,*,#5344,.T.);
#7548=ORIENTED_EDGE('',*,*,#5340,.T.);
#7549=ORIENTED_EDGE('',*,*,#5345,.T.);
#7550=ORIENTED_EDGE('',*,*,#5346,.F.);
#7551=ORIENTED_EDGE('',*,*,#5347,.T.);
#7552=ORIENTED_EDGE('',*,*,#5343,.T.);
#7553=ORIENTED_EDGE('',*,*,#5348,.T.);
#7554=ORIENTED_EDGE('',*,*,#5349,.F.);
#7555=ORIENTED_EDGE('',*,*,#5350,.T.);
#7556=ORIENTED_EDGE('',*,*,#5346,.T.);
#7557=ORIENTED_EDGE('',*,*,#5351,.T.);
#7558=ORIENTED_EDGE('',*,*,#5352,.F.);
#7559=ORIENTED_EDGE('',*,*,#5353,.T.);
#7560=ORIENTED_EDGE('',*,*,#5349,.T.);
#7561=ORIENTED_EDGE('',*,*,#5354,.T.);
#7562=ORIENTED_EDGE('',*,*,#5355,.F.);
#7563=ORIENTED_EDGE('',*,*,#5356,.T.);
#7564=ORIENTED_EDGE('',*,*,#5352,.T.);
#7565=ORIENTED_EDGE('',*,*,#5357,.T.);
#7566=ORIENTED_EDGE('',*,*,#5358,.F.);
#7567=ORIENTED_EDGE('',*,*,#5359,.T.);
#7568=ORIENTED_EDGE('',*,*,#5355,.T.);
#7569=ORIENTED_EDGE('',*,*,#5360,.T.);
#7570=ORIENTED_EDGE('',*,*,#5361,.F.);
#7571=ORIENTED_EDGE('',*,*,#5362,.T.);
#7572=ORIENTED_EDGE('',*,*,#5358,.T.);
#7573=ORIENTED_EDGE('',*,*,#5363,.T.);
#7574=ORIENTED_EDGE('',*,*,#5364,.F.);
#7575=ORIENTED_EDGE('',*,*,#5365,.T.);
#7576=ORIENTED_EDGE('',*,*,#5361,.T.);
#7577=ORIENTED_EDGE('',*,*,#5366,.T.);
#7578=ORIENTED_EDGE('',*,*,#5367,.F.);
#7579=ORIENTED_EDGE('',*,*,#5368,.T.);
#7580=ORIENTED_EDGE('',*,*,#5364,.T.);
#7581=ORIENTED_EDGE('',*,*,#5369,.T.);
#7582=ORIENTED_EDGE('',*,*,#5370,.F.);
#7583=ORIENTED_EDGE('',*,*,#5371,.T.);
#7584=ORIENTED_EDGE('',*,*,#5367,.T.);
#7585=ORIENTED_EDGE('',*,*,#5372,.T.);
#7586=ORIENTED_EDGE('',*,*,#5373,.F.);
#7587=ORIENTED_EDGE('',*,*,#5374,.T.);
#7588=ORIENTED_EDGE('',*,*,#5370,.T.);
#7589=ORIENTED_EDGE('',*,*,#5375,.T.);
#7590=ORIENTED_EDGE('',*,*,#5376,.F.);
#7591=ORIENTED_EDGE('',*,*,#5377,.T.);
#7592=ORIENTED_EDGE('',*,*,#5373,.T.);
#7593=ORIENTED_EDGE('',*,*,#5378,.T.);
#7594=ORIENTED_EDGE('',*,*,#5379,.F.);
#7595=ORIENTED_EDGE('',*,*,#5380,.T.);
#7596=ORIENTED_EDGE('',*,*,#5376,.T.);
#7597=ORIENTED_EDGE('',*,*,#5381,.T.);
#7598=ORIENTED_EDGE('',*,*,#5382,.F.);
#7599=ORIENTED_EDGE('',*,*,#5383,.T.);
#7600=ORIENTED_EDGE('',*,*,#5379,.T.);
#7601=ORIENTED_EDGE('',*,*,#5384,.T.);
#7602=ORIENTED_EDGE('',*,*,#5385,.F.);
#7603=ORIENTED_EDGE('',*,*,#5386,.T.);
#7604=ORIENTED_EDGE('',*,*,#5387,.T.);
#7605=ORIENTED_EDGE('',*,*,#5388,.F.);
#7606=ORIENTED_EDGE('',*,*,#5389,.F.);
#7607=ORIENTED_EDGE('',*,*,#5390,.T.);
#7608=ORIENTED_EDGE('',*,*,#5385,.T.);
#7609=ORIENTED_EDGE('',*,*,#5391,.F.);
#7610=ORIENTED_EDGE('',*,*,#5392,.F.);
#7611=ORIENTED_EDGE('',*,*,#5393,.T.);
#7612=ORIENTED_EDGE('',*,*,#5389,.T.);
#7613=ORIENTED_EDGE('',*,*,#5394,.F.);
#7614=ORIENTED_EDGE('',*,*,#5395,.F.);
#7615=ORIENTED_EDGE('',*,*,#5396,.T.);
#7616=ORIENTED_EDGE('',*,*,#5392,.T.);
#7617=ORIENTED_EDGE('',*,*,#5397,.F.);
#7618=ORIENTED_EDGE('',*,*,#5398,.F.);
#7619=ORIENTED_EDGE('',*,*,#5399,.T.);
#7620=ORIENTED_EDGE('',*,*,#5395,.T.);
#7621=ORIENTED_EDGE('',*,*,#5400,.F.);
#7622=ORIENTED_EDGE('',*,*,#5401,.F.);
#7623=ORIENTED_EDGE('',*,*,#5402,.T.);
#7624=ORIENTED_EDGE('',*,*,#5398,.T.);
#7625=ORIENTED_EDGE('',*,*,#5403,.F.);
#7626=ORIENTED_EDGE('',*,*,#5404,.F.);
#7627=ORIENTED_EDGE('',*,*,#5405,.T.);
#7628=ORIENTED_EDGE('',*,*,#5401,.T.);
#7629=ORIENTED_EDGE('',*,*,#5406,.F.);
#7630=ORIENTED_EDGE('',*,*,#5407,.F.);
#7631=ORIENTED_EDGE('',*,*,#5408,.T.);
#7632=ORIENTED_EDGE('',*,*,#5404,.T.);
#7633=ORIENTED_EDGE('',*,*,#5409,.F.);
#7634=ORIENTED_EDGE('',*,*,#5410,.F.);
#7635=ORIENTED_EDGE('',*,*,#5411,.T.);
#7636=ORIENTED_EDGE('',*,*,#5407,.T.);
#7637=ORIENTED_EDGE('',*,*,#5412,.F.);
#7638=ORIENTED_EDGE('',*,*,#5413,.F.);
#7639=ORIENTED_EDGE('',*,*,#5414,.T.);
#7640=ORIENTED_EDGE('',*,*,#5410,.T.);
#7641=ORIENTED_EDGE('',*,*,#5415,.F.);
#7642=ORIENTED_EDGE('',*,*,#5416,.F.);
#7643=ORIENTED_EDGE('',*,*,#5417,.T.);
#7644=ORIENTED_EDGE('',*,*,#5413,.T.);
#7645=ORIENTED_EDGE('',*,*,#5418,.F.);
#7646=ORIENTED_EDGE('',*,*,#5419,.F.);
#7647=ORIENTED_EDGE('',*,*,#5420,.T.);
#7648=ORIENTED_EDGE('',*,*,#5416,.T.);
#7649=ORIENTED_EDGE('',*,*,#5421,.F.);
#7650=ORIENTED_EDGE('',*,*,#5422,.F.);
#7651=ORIENTED_EDGE('',*,*,#5423,.T.);
#7652=ORIENTED_EDGE('',*,*,#5419,.T.);
#7653=ORIENTED_EDGE('',*,*,#5424,.F.);
#7654=ORIENTED_EDGE('',*,*,#5425,.F.);
#7655=ORIENTED_EDGE('',*,*,#5426,.T.);
#7656=ORIENTED_EDGE('',*,*,#5422,.T.);
#7657=ORIENTED_EDGE('',*,*,#5427,.F.);
#7658=ORIENTED_EDGE('',*,*,#5428,.F.);
#7659=ORIENTED_EDGE('',*,*,#5429,.T.);
#7660=ORIENTED_EDGE('',*,*,#5425,.T.);
#7661=ORIENTED_EDGE('',*,*,#5430,.F.);
#7662=ORIENTED_EDGE('',*,*,#5431,.F.);
#7663=ORIENTED_EDGE('',*,*,#5432,.T.);
#7664=ORIENTED_EDGE('',*,*,#5428,.T.);
#7665=ORIENTED_EDGE('',*,*,#5433,.F.);
#7666=ORIENTED_EDGE('',*,*,#5434,.F.);
#7667=ORIENTED_EDGE('',*,*,#5435,.T.);
#7668=ORIENTED_EDGE('',*,*,#5431,.T.);
#7669=ORIENTED_EDGE('',*,*,#5436,.F.);
#7670=ORIENTED_EDGE('',*,*,#5437,.F.);
#7671=ORIENTED_EDGE('',*,*,#5438,.T.);
#7672=ORIENTED_EDGE('',*,*,#5434,.T.);
#7673=ORIENTED_EDGE('',*,*,#5439,.F.);
#7674=ORIENTED_EDGE('',*,*,#5440,.F.);
#7675=ORIENTED_EDGE('',*,*,#5441,.T.);
#7676=ORIENTED_EDGE('',*,*,#5437,.T.);
#7677=ORIENTED_EDGE('',*,*,#5442,.F.);
#7678=ORIENTED_EDGE('',*,*,#5443,.F.);
#7679=ORIENTED_EDGE('',*,*,#5444,.T.);
#7680=ORIENTED_EDGE('',*,*,#5440,.T.);
#7681=ORIENTED_EDGE('',*,*,#5445,.F.);
#7682=ORIENTED_EDGE('',*,*,#5446,.F.);
#7683=ORIENTED_EDGE('',*,*,#5447,.T.);
#7684=ORIENTED_EDGE('',*,*,#5443,.T.);
#7685=ORIENTED_EDGE('',*,*,#5448,.F.);
#7686=ORIENTED_EDGE('',*,*,#5449,.F.);
#7687=ORIENTED_EDGE('',*,*,#5450,.T.);
#7688=ORIENTED_EDGE('',*,*,#5446,.T.);
#7689=ORIENTED_EDGE('',*,*,#5451,.F.);
#7690=ORIENTED_EDGE('',*,*,#5452,.F.);
#7691=ORIENTED_EDGE('',*,*,#5453,.T.);
#7692=ORIENTED_EDGE('',*,*,#5449,.T.);
#7693=ORIENTED_EDGE('',*,*,#5454,.F.);
#7694=ORIENTED_EDGE('',*,*,#5455,.F.);
#7695=ORIENTED_EDGE('',*,*,#5456,.T.);
#7696=ORIENTED_EDGE('',*,*,#5452,.T.);
#7697=ORIENTED_EDGE('',*,*,#5457,.F.);
#7698=ORIENTED_EDGE('',*,*,#5458,.F.);
#7699=ORIENTED_EDGE('',*,*,#5459,.T.);
#7700=ORIENTED_EDGE('',*,*,#5455,.T.);
#7701=ORIENTED_EDGE('',*,*,#5460,.F.);
#7702=ORIENTED_EDGE('',*,*,#5461,.F.);
#7703=ORIENTED_EDGE('',*,*,#5462,.T.);
#7704=ORIENTED_EDGE('',*,*,#5458,.T.);
#7705=ORIENTED_EDGE('',*,*,#5463,.F.);
#7706=ORIENTED_EDGE('',*,*,#5464,.F.);
#7707=ORIENTED_EDGE('',*,*,#5465,.T.);
#7708=ORIENTED_EDGE('',*,*,#5461,.T.);
#7709=ORIENTED_EDGE('',*,*,#5466,.F.);
#7710=ORIENTED_EDGE('',*,*,#5467,.F.);
#7711=ORIENTED_EDGE('',*,*,#5468,.T.);
#7712=ORIENTED_EDGE('',*,*,#5464,.T.);
#7713=ORIENTED_EDGE('',*,*,#5469,.F.);
#7714=ORIENTED_EDGE('',*,*,#5470,.F.);
#7715=ORIENTED_EDGE('',*,*,#5471,.T.);
#7716=ORIENTED_EDGE('',*,*,#5467,.T.);
#7717=ORIENTED_EDGE('',*,*,#5472,.F.);
#7718=ORIENTED_EDGE('',*,*,#5473,.F.);
#7719=ORIENTED_EDGE('',*,*,#5474,.T.);
#7720=ORIENTED_EDGE('',*,*,#5470,.T.);
#7721=ORIENTED_EDGE('',*,*,#5475,.F.);
#7722=ORIENTED_EDGE('',*,*,#5476,.F.);
#7723=ORIENTED_EDGE('',*,*,#5387,.F.);
#7724=ORIENTED_EDGE('',*,*,#5477,.F.);
#7725=ORIENTED_EDGE('',*,*,#5478,.F.);
#7726=ORIENTED_EDGE('',*,*,#5479,.F.);
#7727=ORIENTED_EDGE('',*,*,#5480,.T.);
#7728=ORIENTED_EDGE('',*,*,#5481,.F.);
#7729=ORIENTED_EDGE('',*,*,#5480,.F.);
#7730=ORIENTED_EDGE('',*,*,#5477,.T.);
#7731=ORIENTED_EDGE('',*,*,#5386,.F.);
#7732=ORIENTED_EDGE('',*,*,#5390,.F.);
#7733=ORIENTED_EDGE('',*,*,#5393,.F.);
#7734=ORIENTED_EDGE('',*,*,#5396,.F.);
#7735=ORIENTED_EDGE('',*,*,#5399,.F.);
#7736=ORIENTED_EDGE('',*,*,#5402,.F.);
#7737=ORIENTED_EDGE('',*,*,#5405,.F.);
#7738=ORIENTED_EDGE('',*,*,#5408,.F.);
#7739=ORIENTED_EDGE('',*,*,#5411,.F.);
#7740=ORIENTED_EDGE('',*,*,#5414,.F.);
#7741=ORIENTED_EDGE('',*,*,#5417,.F.);
#7742=ORIENTED_EDGE('',*,*,#5420,.F.);
#7743=ORIENTED_EDGE('',*,*,#5423,.F.);
#7744=ORIENTED_EDGE('',*,*,#5426,.F.);
#7745=ORIENTED_EDGE('',*,*,#5429,.F.);
#7746=ORIENTED_EDGE('',*,*,#5432,.F.);
#7747=ORIENTED_EDGE('',*,*,#5435,.F.);
#7748=ORIENTED_EDGE('',*,*,#5438,.F.);
#7749=ORIENTED_EDGE('',*,*,#5441,.F.);
#7750=ORIENTED_EDGE('',*,*,#5444,.F.);
#7751=ORIENTED_EDGE('',*,*,#5447,.F.);
#7752=ORIENTED_EDGE('',*,*,#5450,.F.);
#7753=ORIENTED_EDGE('',*,*,#5453,.F.);
#7754=ORIENTED_EDGE('',*,*,#5456,.F.);
#7755=ORIENTED_EDGE('',*,*,#5459,.F.);
#7756=ORIENTED_EDGE('',*,*,#5462,.F.);
#7757=ORIENTED_EDGE('',*,*,#5465,.F.);
#7758=ORIENTED_EDGE('',*,*,#5468,.F.);
#7759=ORIENTED_EDGE('',*,*,#5471,.F.);
#7760=ORIENTED_EDGE('',*,*,#5474,.F.);
#7761=ORIENTED_EDGE('',*,*,#5482,.F.);
#7762=ORIENTED_EDGE('',*,*,#5483,.F.);
#7763=ORIENTED_EDGE('',*,*,#5295,.F.);
#7764=ORIENTED_EDGE('',*,*,#5299,.F.);
#7765=ORIENTED_EDGE('',*,*,#5302,.F.);
#7766=ORIENTED_EDGE('',*,*,#5305,.F.);
#7767=ORIENTED_EDGE('',*,*,#5308,.F.);
#7768=ORIENTED_EDGE('',*,*,#5311,.F.);
#7769=ORIENTED_EDGE('',*,*,#5314,.F.);
#7770=ORIENTED_EDGE('',*,*,#5317,.F.);
#7771=ORIENTED_EDGE('',*,*,#5320,.F.);
#7772=ORIENTED_EDGE('',*,*,#5323,.F.);
#7773=ORIENTED_EDGE('',*,*,#5326,.F.);
#7774=ORIENTED_EDGE('',*,*,#5329,.F.);
#7775=ORIENTED_EDGE('',*,*,#5332,.F.);
#7776=ORIENTED_EDGE('',*,*,#5335,.F.);
#7777=ORIENTED_EDGE('',*,*,#5338,.F.);
#7778=ORIENTED_EDGE('',*,*,#5341,.F.);
#7779=ORIENTED_EDGE('',*,*,#5344,.F.);
#7780=ORIENTED_EDGE('',*,*,#5347,.F.);
#7781=ORIENTED_EDGE('',*,*,#5350,.F.);
#7782=ORIENTED_EDGE('',*,*,#5353,.F.);
#7783=ORIENTED_EDGE('',*,*,#5356,.F.);
#7784=ORIENTED_EDGE('',*,*,#5359,.F.);
#7785=ORIENTED_EDGE('',*,*,#5362,.F.);
#7786=ORIENTED_EDGE('',*,*,#5365,.F.);
#7787=ORIENTED_EDGE('',*,*,#5368,.F.);
#7788=ORIENTED_EDGE('',*,*,#5371,.F.);
#7789=ORIENTED_EDGE('',*,*,#5374,.F.);
#7790=ORIENTED_EDGE('',*,*,#5377,.F.);
#7791=ORIENTED_EDGE('',*,*,#5380,.F.);
#7792=ORIENTED_EDGE('',*,*,#5383,.F.);
#7793=ORIENTED_EDGE('',*,*,#5484,.F.);
#7794=ORIENTED_EDGE('',*,*,#5473,.T.);
#7795=ORIENTED_EDGE('',*,*,#5485,.F.);
#7796=ORIENTED_EDGE('',*,*,#5486,.F.);
#7797=ORIENTED_EDGE('',*,*,#5482,.T.);
#7798=ORIENTED_EDGE('',*,*,#5476,.T.);
#7799=ORIENTED_EDGE('',*,*,#5479,.T.);
#7800=ORIENTED_EDGE('',*,*,#5487,.F.);
#7801=ORIENTED_EDGE('',*,*,#5384,.F.);
#7802=ORIENTED_EDGE('',*,*,#5381,.F.);
#7803=ORIENTED_EDGE('',*,*,#5378,.F.);
#7804=ORIENTED_EDGE('',*,*,#5375,.F.);
#7805=ORIENTED_EDGE('',*,*,#5372,.F.);
#7806=ORIENTED_EDGE('',*,*,#5369,.F.);
#7807=ORIENTED_EDGE('',*,*,#5366,.F.);
#7808=ORIENTED_EDGE('',*,*,#5363,.F.);
#7809=ORIENTED_EDGE('',*,*,#5360,.F.);
#7810=ORIENTED_EDGE('',*,*,#5357,.F.);
#7811=ORIENTED_EDGE('',*,*,#5354,.F.);
#7812=ORIENTED_EDGE('',*,*,#5351,.F.);
#7813=ORIENTED_EDGE('',*,*,#5348,.F.);
#7814=ORIENTED_EDGE('',*,*,#5345,.F.);
#7815=ORIENTED_EDGE('',*,*,#5342,.F.);
#7816=ORIENTED_EDGE('',*,*,#5339,.F.);
#7817=ORIENTED_EDGE('',*,*,#5336,.F.);
#7818=ORIENTED_EDGE('',*,*,#5333,.F.);
#7819=ORIENTED_EDGE('',*,*,#5330,.F.);
#7820=ORIENTED_EDGE('',*,*,#5327,.F.);
#7821=ORIENTED_EDGE('',*,*,#5324,.F.);
#7822=ORIENTED_EDGE('',*,*,#5321,.F.);
#7823=ORIENTED_EDGE('',*,*,#5318,.F.);
#7824=ORIENTED_EDGE('',*,*,#5315,.F.);
#7825=ORIENTED_EDGE('',*,*,#5312,.F.);
#7826=ORIENTED_EDGE('',*,*,#5309,.F.);
#7827=ORIENTED_EDGE('',*,*,#5306,.F.);
#7828=ORIENTED_EDGE('',*,*,#5303,.F.);
#7829=ORIENTED_EDGE('',*,*,#5300,.F.);
#7830=ORIENTED_EDGE('',*,*,#5297,.F.);
#7831=ORIENTED_EDGE('',*,*,#5488,.F.);
#7832=ORIENTED_EDGE('',*,*,#5485,.T.);
#7833=ORIENTED_EDGE('',*,*,#5475,.T.);
#7834=ORIENTED_EDGE('',*,*,#5472,.T.);
#7835=ORIENTED_EDGE('',*,*,#5469,.T.);
#7836=ORIENTED_EDGE('',*,*,#5466,.T.);
#7837=ORIENTED_EDGE('',*,*,#5463,.T.);
#7838=ORIENTED_EDGE('',*,*,#5460,.T.);
#7839=ORIENTED_EDGE('',*,*,#5457,.T.);
#7840=ORIENTED_EDGE('',*,*,#5454,.T.);
#7841=ORIENTED_EDGE('',*,*,#5451,.T.);
#7842=ORIENTED_EDGE('',*,*,#5448,.T.);
#7843=ORIENTED_EDGE('',*,*,#5445,.T.);
#7844=ORIENTED_EDGE('',*,*,#5442,.T.);
#7845=ORIENTED_EDGE('',*,*,#5439,.T.);
#7846=ORIENTED_EDGE('',*,*,#5436,.T.);
#7847=ORIENTED_EDGE('',*,*,#5433,.T.);
#7848=ORIENTED_EDGE('',*,*,#5430,.T.);
#7849=ORIENTED_EDGE('',*,*,#5427,.T.);
#7850=ORIENTED_EDGE('',*,*,#5424,.T.);
#7851=ORIENTED_EDGE('',*,*,#5421,.T.);
#7852=ORIENTED_EDGE('',*,*,#5418,.T.);
#7853=ORIENTED_EDGE('',*,*,#5415,.T.);
#7854=ORIENTED_EDGE('',*,*,#5412,.T.);
#7855=ORIENTED_EDGE('',*,*,#5409,.T.);
#7856=ORIENTED_EDGE('',*,*,#5406,.T.);
#7857=ORIENTED_EDGE('',*,*,#5403,.T.);
#7858=ORIENTED_EDGE('',*,*,#5400,.T.);
#7859=ORIENTED_EDGE('',*,*,#5397,.T.);
#7860=ORIENTED_EDGE('',*,*,#5394,.T.);
#7861=ORIENTED_EDGE('',*,*,#5391,.T.);
#7862=ORIENTED_EDGE('',*,*,#5388,.T.);
#7863=ORIENTED_EDGE('',*,*,#5382,.T.);
#7864=ORIENTED_EDGE('',*,*,#5487,.T.);
#7865=ORIENTED_EDGE('',*,*,#5478,.T.);
#7866=ORIENTED_EDGE('',*,*,#5484,.T.);
#7867=ORIENTED_EDGE('',*,*,#5489,.F.);
#7868=ORIENTED_EDGE('',*,*,#5490,.T.);
#7869=ORIENTED_EDGE('',*,*,#5491,.T.);
#7870=ORIENTED_EDGE('',*,*,#5492,.F.);
#7871=ORIENTED_EDGE('',*,*,#5493,.F.);
#7872=ORIENTED_EDGE('',*,*,#5494,.T.);
#7873=ORIENTED_EDGE('',*,*,#5495,.T.);
#7874=ORIENTED_EDGE('',*,*,#5490,.F.);
#7875=ORIENTED_EDGE('',*,*,#5496,.F.);
#7876=ORIENTED_EDGE('',*,*,#5497,.T.);
#7877=ORIENTED_EDGE('',*,*,#5498,.T.);
#7878=ORIENTED_EDGE('',*,*,#5494,.F.);
#7879=ORIENTED_EDGE('',*,*,#5499,.F.);
#7880=ORIENTED_EDGE('',*,*,#5500,.T.);
#7881=ORIENTED_EDGE('',*,*,#5501,.T.);
#7882=ORIENTED_EDGE('',*,*,#5497,.F.);
#7883=ORIENTED_EDGE('',*,*,#5502,.F.);
#7884=ORIENTED_EDGE('',*,*,#5503,.T.);
#7885=ORIENTED_EDGE('',*,*,#5504,.T.);
#7886=ORIENTED_EDGE('',*,*,#5500,.F.);
#7887=ORIENTED_EDGE('',*,*,#5505,.F.);
#7888=ORIENTED_EDGE('',*,*,#5492,.T.);
#7889=ORIENTED_EDGE('',*,*,#5506,.T.);
#7890=ORIENTED_EDGE('',*,*,#5503,.F.);
#7891=ORIENTED_EDGE('',*,*,#5506,.F.);
#7892=ORIENTED_EDGE('',*,*,#5491,.F.);
#7893=ORIENTED_EDGE('',*,*,#5495,.F.);
#7894=ORIENTED_EDGE('',*,*,#5498,.F.);
#7895=ORIENTED_EDGE('',*,*,#5501,.F.);
#7896=ORIENTED_EDGE('',*,*,#5504,.F.);
#7897=ORIENTED_EDGE('',*,*,#5507,.T.);
#7898=ORIENTED_EDGE('',*,*,#5483,.T.);
#7899=ORIENTED_EDGE('',*,*,#5486,.T.);
#7900=ORIENTED_EDGE('',*,*,#5488,.T.);
#7901=ORIENTED_EDGE('',*,*,#5296,.F.);
#7902=ORIENTED_EDGE('',*,*,#5507,.F.);
#7903=ORIENTED_EDGE('',*,*,#5508,.T.);
#7904=ORIENTED_EDGE('',*,*,#5509,.T.);
#7905=ORIENTED_EDGE('',*,*,#5508,.F.);
#7906=ORIENTED_EDGE('',*,*,#5509,.F.);
#7907=ORIENTED_EDGE('',*,*,#5489,.T.);
#7908=ORIENTED_EDGE('',*,*,#5505,.T.);
#7909=ORIENTED_EDGE('',*,*,#5502,.T.);
#7910=ORIENTED_EDGE('',*,*,#5499,.T.);
#7911=ORIENTED_EDGE('',*,*,#5496,.T.);
#7912=ORIENTED_EDGE('',*,*,#5493,.T.);
#7913=ORIENTED_EDGE('',*,*,#5481,.T.);
#7914=ORIENTED_EDGE('',*,*,#5510,.T.);
#7915=ORIENTED_EDGE('',*,*,#5511,.F.);
#7916=ORIENTED_EDGE('',*,*,#5512,.T.);
#7917=ORIENTED_EDGE('',*,*,#5513,.T.);
#7918=ORIENTED_EDGE('',*,*,#5514,.T.);
#7919=ORIENTED_EDGE('',*,*,#5515,.F.);
#7920=ORIENTED_EDGE('',*,*,#5510,.F.);
#7921=ORIENTED_EDGE('',*,*,#5516,.T.);
#7922=ORIENTED_EDGE('',*,*,#5517,.T.);
#7923=ORIENTED_EDGE('',*,*,#5518,.T.);
#7924=ORIENTED_EDGE('',*,*,#5513,.F.);
#7925=ORIENTED_EDGE('',*,*,#5519,.T.);
#7926=ORIENTED_EDGE('',*,*,#5520,.T.);
#7927=ORIENTED_EDGE('',*,*,#5521,.T.);
#7928=ORIENTED_EDGE('',*,*,#5517,.F.);
#7929=ORIENTED_EDGE('',*,*,#5522,.T.);
#7930=ORIENTED_EDGE('',*,*,#5523,.F.);
#7931=ORIENTED_EDGE('',*,*,#5524,.T.);
#7932=ORIENTED_EDGE('',*,*,#5525,.F.);
#7933=ORIENTED_EDGE('',*,*,#5526,.T.);
#7934=ORIENTED_EDGE('',*,*,#5527,.T.);
#7935=ORIENTED_EDGE('',*,*,#5528,.T.);
#7936=ORIENTED_EDGE('',*,*,#5529,.F.);
#7937=ORIENTED_EDGE('',*,*,#5530,.F.);
#7938=ORIENTED_EDGE('',*,*,#5531,.T.);
#7939=ORIENTED_EDGE('',*,*,#5532,.T.);
#7940=ORIENTED_EDGE('',*,*,#5527,.F.);
#7941=ORIENTED_EDGE('',*,*,#5533,.F.);
#7942=ORIENTED_EDGE('',*,*,#5534,.T.);
#7943=ORIENTED_EDGE('',*,*,#5535,.T.);
#7944=ORIENTED_EDGE('',*,*,#5531,.F.);
#7945=ORIENTED_EDGE('',*,*,#5536,.F.);
#7946=ORIENTED_EDGE('',*,*,#5537,.T.);
#7947=ORIENTED_EDGE('',*,*,#5538,.T.);
#7948=ORIENTED_EDGE('',*,*,#5534,.F.);
#7949=ORIENTED_EDGE('',*,*,#5539,.F.);
#7950=ORIENTED_EDGE('',*,*,#5540,.F.);
#7951=ORIENTED_EDGE('',*,*,#5541,.F.);
#7952=ORIENTED_EDGE('',*,*,#5542,.F.);
#7953=ORIENTED_EDGE('',*,*,#5543,.T.);
#7954=ORIENTED_EDGE('',*,*,#5540,.T.);
#7955=ORIENTED_EDGE('',*,*,#5544,.T.);
#7956=ORIENTED_EDGE('',*,*,#5537,.F.);
#7957=ORIENTED_EDGE('',*,*,#5545,.F.);
#7958=ORIENTED_EDGE('',*,*,#5546,.F.);
#7959=ORIENTED_EDGE('',*,*,#5528,.F.);
#7960=ORIENTED_EDGE('',*,*,#5532,.F.);
#7961=ORIENTED_EDGE('',*,*,#5535,.F.);
#7962=ORIENTED_EDGE('',*,*,#5538,.F.);
#7963=ORIENTED_EDGE('',*,*,#5544,.F.);
#7964=ORIENTED_EDGE('',*,*,#5543,.F.);
#7965=ORIENTED_EDGE('',*,*,#5547,.F.);
#7966=ORIENTED_EDGE('',*,*,#5524,.F.);
#7967=ORIENTED_EDGE('',*,*,#5548,.F.);
#7968=ORIENTED_EDGE('',*,*,#5522,.F.);
#7969=ORIENTED_EDGE('',*,*,#5519,.F.);
#7970=ORIENTED_EDGE('',*,*,#5516,.F.);
#7971=ORIENTED_EDGE('',*,*,#5512,.F.);
#7972=ORIENTED_EDGE('',*,*,#5549,.F.);
#7973=ORIENTED_EDGE('',*,*,#5514,.F.);
#7974=ORIENTED_EDGE('',*,*,#5518,.F.);
#7975=ORIENTED_EDGE('',*,*,#5521,.F.);
#7976=ORIENTED_EDGE('',*,*,#5550,.F.);
#7977=ORIENTED_EDGE('',*,*,#5526,.F.);
#7978=ORIENTED_EDGE('',*,*,#5551,.F.);
#7979=ORIENTED_EDGE('',*,*,#5541,.T.);
#7980=ORIENTED_EDGE('',*,*,#5545,.T.);
#7981=ORIENTED_EDGE('',*,*,#5539,.T.);
#7982=ORIENTED_EDGE('',*,*,#5536,.T.);
#7983=ORIENTED_EDGE('',*,*,#5533,.T.);
#7984=ORIENTED_EDGE('',*,*,#5530,.T.);
#7985=ORIENTED_EDGE('',*,*,#5552,.T.);
#7986=ORIENTED_EDGE('',*,*,#5553,.T.);
#7987=ORIENTED_EDGE('',*,*,#5554,.T.);
#7988=ORIENTED_EDGE('',*,*,#5555,.T.);
#7989=ORIENTED_EDGE('',*,*,#5556,.T.);
#7990=ORIENTED_EDGE('',*,*,#5557,.T.);
#7991=ORIENTED_EDGE('',*,*,#5547,.T.);
#7992=ORIENTED_EDGE('',*,*,#5542,.T.);
#7993=ORIENTED_EDGE('',*,*,#5551,.T.);
#7994=ORIENTED_EDGE('',*,*,#5525,.T.);
#7995=ORIENTED_EDGE('',*,*,#5523,.T.);
#7996=ORIENTED_EDGE('',*,*,#5550,.T.);
#7997=ORIENTED_EDGE('',*,*,#5520,.F.);
#7998=ORIENTED_EDGE('',*,*,#5548,.T.);
#7999=ORIENTED_EDGE('',*,*,#5558,.T.);
#8000=ORIENTED_EDGE('',*,*,#5559,.T.);
#8001=ORIENTED_EDGE('',*,*,#5557,.F.);
#8002=ORIENTED_EDGE('',*,*,#5560,.F.);
#8003=ORIENTED_EDGE('',*,*,#5561,.T.);
#8004=ORIENTED_EDGE('',*,*,#5560,.T.);
#8005=ORIENTED_EDGE('',*,*,#5556,.F.);
#8006=ORIENTED_EDGE('',*,*,#5562,.F.);
#8007=ORIENTED_EDGE('',*,*,#5563,.T.);
#8008=ORIENTED_EDGE('',*,*,#5562,.T.);
#8009=ORIENTED_EDGE('',*,*,#5555,.F.);
#8010=ORIENTED_EDGE('',*,*,#5564,.F.);
#8011=ORIENTED_EDGE('',*,*,#5565,.T.);
#8012=ORIENTED_EDGE('',*,*,#5564,.T.);
#8013=ORIENTED_EDGE('',*,*,#5554,.F.);
#8014=ORIENTED_EDGE('',*,*,#5566,.F.);
#8015=ORIENTED_EDGE('',*,*,#5567,.T.);
#8016=ORIENTED_EDGE('',*,*,#5566,.T.);
#8017=ORIENTED_EDGE('',*,*,#5553,.F.);
#8018=ORIENTED_EDGE('',*,*,#5568,.F.);
#8019=ORIENTED_EDGE('',*,*,#5569,.T.);
#8020=ORIENTED_EDGE('',*,*,#5568,.T.);
#8021=ORIENTED_EDGE('',*,*,#5552,.F.);
#8022=ORIENTED_EDGE('',*,*,#5559,.F.);
#8023=ORIENTED_EDGE('',*,*,#5569,.F.);
#8024=ORIENTED_EDGE('',*,*,#5558,.F.);
#8025=ORIENTED_EDGE('',*,*,#5561,.F.);
#8026=ORIENTED_EDGE('',*,*,#5563,.F.);
#8027=ORIENTED_EDGE('',*,*,#5565,.F.);
#8028=ORIENTED_EDGE('',*,*,#5567,.F.);
#8029=ORIENTED_EDGE('',*,*,#5546,.T.);
#8030=ORIENTED_EDGE('',*,*,#5511,.T.);
#8031=ORIENTED_EDGE('',*,*,#5515,.T.);
#8032=ORIENTED_EDGE('',*,*,#5549,.T.);
#8033=ORIENTED_EDGE('',*,*,#5529,.T.);
#8034=ORIENTED_EDGE('',*,*,#5570,.F.);
#8035=ORIENTED_EDGE('',*,*,#5571,.T.);
#8036=ORIENTED_EDGE('',*,*,#5572,.F.);
#8037=ORIENTED_EDGE('',*,*,#5571,.F.);
#8038=ORIENTED_EDGE('',*,*,#5573,.F.);
#8039=ORIENTED_EDGE('',*,*,#5574,.T.);
#8040=ORIENTED_EDGE('',*,*,#5575,.F.);
#8041=ORIENTED_EDGE('',*,*,#5574,.F.);
#8042=ORIENTED_EDGE('',*,*,#5576,.T.);
#8043=ORIENTED_EDGE('',*,*,#5577,.T.);
#8044=ORIENTED_EDGE('',*,*,#5578,.F.);
#8045=ORIENTED_EDGE('',*,*,#5579,.T.);
#8046=ORIENTED_EDGE('',*,*,#5576,.F.);
#8047=ORIENTED_EDGE('',*,*,#5579,.F.);
#8048=ORIENTED_EDGE('',*,*,#5578,.T.);
#8049=ORIENTED_EDGE('',*,*,#5580,.T.);
#8050=ORIENTED_EDGE('',*,*,#5581,.T.);
#8051=ORIENTED_EDGE('',*,*,#5582,.F.);
#8052=ORIENTED_EDGE('',*,*,#5583,.T.);
#8053=ORIENTED_EDGE('',*,*,#5580,.F.);
#8054=ORIENTED_EDGE('',*,*,#5583,.F.);
#8055=ORIENTED_EDGE('',*,*,#5582,.T.);
#8056=ORIENTED_EDGE('',*,*,#5584,.T.);
#8057=ORIENTED_EDGE('',*,*,#5585,.T.);
#8058=ORIENTED_EDGE('',*,*,#5586,.F.);
#8059=ORIENTED_EDGE('',*,*,#5587,.T.);
#8060=ORIENTED_EDGE('',*,*,#5584,.F.);
#8061=ORIENTED_EDGE('',*,*,#5587,.F.);
#8062=ORIENTED_EDGE('',*,*,#5586,.T.);
#8063=ORIENTED_EDGE('',*,*,#5588,.T.);
#8064=ORIENTED_EDGE('',*,*,#5589,.T.);
#8065=ORIENTED_EDGE('',*,*,#5590,.F.);
#8066=ORIENTED_EDGE('',*,*,#5591,.T.);
#8067=ORIENTED_EDGE('',*,*,#5588,.F.);
#8068=ORIENTED_EDGE('',*,*,#5591,.F.);
#8069=ORIENTED_EDGE('',*,*,#5590,.T.);
#8070=ORIENTED_EDGE('',*,*,#5577,.F.);
#8071=ORIENTED_EDGE('',*,*,#5592,.T.);
#8072=ORIENTED_EDGE('',*,*,#5593,.F.);
#8073=ORIENTED_EDGE('',*,*,#5592,.F.);
#8074=ORIENTED_EDGE('',*,*,#5581,.F.);
#8075=ORIENTED_EDGE('',*,*,#5594,.T.);
#8076=ORIENTED_EDGE('',*,*,#5595,.F.);
#8077=ORIENTED_EDGE('',*,*,#5594,.F.);
#8078=ORIENTED_EDGE('',*,*,#5585,.F.);
#8079=ORIENTED_EDGE('',*,*,#5596,.T.);
#8080=ORIENTED_EDGE('',*,*,#5597,.F.);
#8081=ORIENTED_EDGE('',*,*,#5596,.F.);
#8082=ORIENTED_EDGE('',*,*,#5589,.F.);
#8083=ORIENTED_EDGE('',*,*,#5598,.T.);
#8084=ORIENTED_EDGE('',*,*,#5599,.F.);
#8085=ORIENTED_EDGE('',*,*,#5598,.F.);
#8086=ORIENTED_EDGE('',*,*,#5600,.T.);
#8087=ORIENTED_EDGE('',*,*,#5601,.T.);
#8088=ORIENTED_EDGE('',*,*,#5602,.T.);
#8089=ORIENTED_EDGE('',*,*,#5603,.T.);
#8090=ORIENTED_EDGE('',*,*,#5604,.T.);
#8091=ORIENTED_EDGE('',*,*,#5605,.T.);
#8092=ORIENTED_EDGE('',*,*,#5600,.F.);
#8093=ORIENTED_EDGE('',*,*,#5606,.T.);
#8094=ORIENTED_EDGE('',*,*,#5607,.T.);
#8095=ORIENTED_EDGE('',*,*,#5608,.T.);
#8096=ORIENTED_EDGE('',*,*,#5604,.F.);
#8097=ORIENTED_EDGE('',*,*,#5609,.T.);
#8098=ORIENTED_EDGE('',*,*,#5610,.T.);
#8099=ORIENTED_EDGE('',*,*,#5611,.T.);
#8100=ORIENTED_EDGE('',*,*,#5607,.F.);
#8101=ORIENTED_EDGE('',*,*,#5612,.T.);
#8102=ORIENTED_EDGE('',*,*,#5613,.T.);
#8103=ORIENTED_EDGE('',*,*,#5614,.T.);
#8104=ORIENTED_EDGE('',*,*,#5610,.F.);
#8105=ORIENTED_EDGE('',*,*,#5615,.T.);
#8106=ORIENTED_EDGE('',*,*,#5616,.T.);
#8107=ORIENTED_EDGE('',*,*,#5617,.T.);
#8108=ORIENTED_EDGE('',*,*,#5613,.F.);
#8109=ORIENTED_EDGE('',*,*,#5618,.T.);
#8110=ORIENTED_EDGE('',*,*,#5619,.T.);
#8111=ORIENTED_EDGE('',*,*,#5620,.T.);
#8112=ORIENTED_EDGE('',*,*,#5616,.F.);
#8113=ORIENTED_EDGE('',*,*,#5621,.T.);
#8114=ORIENTED_EDGE('',*,*,#5602,.F.);
#8115=ORIENTED_EDGE('',*,*,#5622,.T.);
#8116=ORIENTED_EDGE('',*,*,#5619,.F.);
#8117=ORIENTED_EDGE('',*,*,#5623,.T.);
#8118=ORIENTED_EDGE('',*,*,#5617,.F.);
#8119=ORIENTED_EDGE('',*,*,#5624,.F.);
#8120=ORIENTED_EDGE('',*,*,#5625,.F.);
#8121=ORIENTED_EDGE('',*,*,#5626,.F.);
#8122=ORIENTED_EDGE('',*,*,#5620,.F.);
#8123=ORIENTED_EDGE('',*,*,#5627,.T.);
#8124=ORIENTED_EDGE('',*,*,#5628,.T.);
#8125=ORIENTED_EDGE('',*,*,#5624,.T.);
#8126=ORIENTED_EDGE('',*,*,#5622,.F.);
#8127=ORIENTED_EDGE('',*,*,#5629,.F.);
#8128=ORIENTED_EDGE('',*,*,#5630,.F.);
#8129=ORIENTED_EDGE('',*,*,#5627,.F.);
#8130=ORIENTED_EDGE('',*,*,#5601,.F.);
#8131=ORIENTED_EDGE('',*,*,#5631,.T.);
#8132=ORIENTED_EDGE('',*,*,#5632,.T.);
#8133=ORIENTED_EDGE('',*,*,#5629,.T.);
#8134=ORIENTED_EDGE('',*,*,#5603,.F.);
#8135=ORIENTED_EDGE('',*,*,#5623,.F.);
#8136=ORIENTED_EDGE('',*,*,#5621,.F.);
#8137=ORIENTED_EDGE('',*,*,#5618,.F.);
#8138=ORIENTED_EDGE('',*,*,#5615,.F.);
#8139=ORIENTED_EDGE('',*,*,#5612,.F.);
#8140=ORIENTED_EDGE('',*,*,#5609,.F.);
#8141=ORIENTED_EDGE('',*,*,#5606,.F.);
#8142=ORIENTED_EDGE('',*,*,#5570,.T.);
#8143=ORIENTED_EDGE('',*,*,#5573,.T.);
#8144=ORIENTED_EDGE('',*,*,#5605,.F.);
#8145=ORIENTED_EDGE('',*,*,#5633,.F.);
#8146=ORIENTED_EDGE('',*,*,#5634,.F.);
#8147=ORIENTED_EDGE('',*,*,#5631,.F.);
#8148=ORIENTED_EDGE('',*,*,#5614,.F.);
#8149=ORIENTED_EDGE('',*,*,#5626,.T.);
#8150=ORIENTED_EDGE('',*,*,#5635,.T.);
#8151=ORIENTED_EDGE('',*,*,#5636,.T.);
#8152=ORIENTED_EDGE('',*,*,#5608,.F.);
#8153=ORIENTED_EDGE('',*,*,#5637,.T.);
#8154=ORIENTED_EDGE('',*,*,#5638,.T.);
#8155=ORIENTED_EDGE('',*,*,#5633,.T.);
#8156=ORIENTED_EDGE('',*,*,#5632,.F.);
#8157=ORIENTED_EDGE('',*,*,#5634,.T.);
#8158=ORIENTED_EDGE('',*,*,#5638,.F.);
#8159=ORIENTED_EDGE('',*,*,#5639,.T.);
#8160=ORIENTED_EDGE('',*,*,#5635,.F.);
#8161=ORIENTED_EDGE('',*,*,#5625,.T.);
#8162=ORIENTED_EDGE('',*,*,#5628,.F.);
#8163=ORIENTED_EDGE('',*,*,#5630,.T.);
#8164=ORIENTED_EDGE('',*,*,#5572,.T.);
#8165=ORIENTED_EDGE('',*,*,#5575,.T.);
#8166=ORIENTED_EDGE('',*,*,#5593,.T.);
#8167=ORIENTED_EDGE('',*,*,#5595,.T.);
#8168=ORIENTED_EDGE('',*,*,#5597,.T.);
#8169=ORIENTED_EDGE('',*,*,#5599,.T.);
#8170=ORIENTED_EDGE('',*,*,#5611,.F.);
#8171=ORIENTED_EDGE('',*,*,#5636,.F.);
#8172=ORIENTED_EDGE('',*,*,#5639,.F.);
#8173=ORIENTED_EDGE('',*,*,#5637,.F.);
#8174=ORIENTED_EDGE('',*,*,#5640,.F.);
#8175=ORIENTED_EDGE('',*,*,#5641,.T.);
#8176=ORIENTED_EDGE('',*,*,#5642,.T.);
#8177=ORIENTED_EDGE('',*,*,#5641,.F.);
#8178=ORIENTED_EDGE('',*,*,#5643,.F.);
#8179=ORIENTED_EDGE('',*,*,#5644,.T.);
#8180=ORIENTED_EDGE('',*,*,#5645,.T.);
#8181=ORIENTED_EDGE('',*,*,#5644,.F.);
#8182=ORIENTED_EDGE('',*,*,#5643,.T.);
#8183=ORIENTED_EDGE('',*,*,#5640,.T.);
#8184=ORIENTED_EDGE('',*,*,#5645,.F.);
#8185=ORIENTED_EDGE('',*,*,#5642,.F.);
#8186=CYLINDRICAL_SURFACE('',#8914,0.17);
#8187=CYLINDRICAL_SURFACE('',#8917,0.17);
#8188=CYLINDRICAL_SURFACE('',#8920,0.41);
#8189=CYLINDRICAL_SURFACE('',#9047,1.4);
#8190=CYLINDRICAL_SURFACE('',#9057,1.4);
#8191=CYLINDRICAL_SURFACE('',#9059,0.3);
#8192=CYLINDRICAL_SURFACE('',#9066,0.4);
#8193=CYLINDRICAL_SURFACE('',#9071,0.6);
#8194=CYLINDRICAL_SURFACE('',#9074,0.4);
#8195=CYLINDRICAL_SURFACE('',#9082,0.3);
#8196=CYLINDRICAL_SURFACE('',#9084,0.6);
#8197=CYLINDRICAL_SURFACE('',#9089,0.25);
#8198=CYLINDRICAL_SURFACE('',#9091,0.25);
#8199=CYLINDRICAL_SURFACE('',#9093,0.25);
#8200=CYLINDRICAL_SURFACE('',#9095,0.25);
#8201=CYLINDRICAL_SURFACE('',#9101,0.15);
#8202=CYLINDRICAL_SURFACE('',#9103,0.15);
#8203=CYLINDRICAL_SURFACE('',#9106,0.15);
#8204=CYLINDRICAL_SURFACE('',#9109,0.15);
#8205=CYLINDRICAL_SURFACE('',#9111,0.3);
#8206=CYLINDRICAL_SURFACE('',#9116,0.3);
#8207=CYLINDRICAL_SURFACE('',#9121,0.17);
#8208=CYLINDRICAL_SURFACE('',#9123,0.17);
#8209=CYLINDRICAL_SURFACE('',#9147,0.4);
#8210=CYLINDRICAL_SURFACE('',#9148,0.4);
#8211=CYLINDRICAL_SURFACE('',#9171,0.1);
#8212=CYLINDRICAL_SURFACE('',#9175,0.1);
#8213=CYLINDRICAL_SURFACE('',#9189,0.3);
#8214=CYLINDRICAL_SURFACE('',#9194,0.3);
#8215=CYLINDRICAL_SURFACE('',#9199,0.25);
#8216=CYLINDRICAL_SURFACE('',#9201,0.25);
#8217=CYLINDRICAL_SURFACE('',#9203,0.25);
#8218=CYLINDRICAL_SURFACE('',#9205,0.25);
#8219=CYLINDRICAL_SURFACE('',#9227,0.15);
#8220=CYLINDRICAL_SURFACE('',#9229,0.15);
#8221=CYLINDRICAL_SURFACE('',#9232,0.15);
#8222=CYLINDRICAL_SURFACE('',#9235,0.15);
#8223=CYLINDRICAL_SURFACE('',#9237,0.17);
#8224=CYLINDRICAL_SURFACE('',#9239,0.17);
#8225=CYLINDRICAL_SURFACE('',#9263,0.4);
#8226=CYLINDRICAL_SURFACE('',#9264,0.4);
#8227=CYLINDRICAL_SURFACE('',#9287,0.1);
#8228=CYLINDRICAL_SURFACE('',#9291,0.1);
#8229=CYLINDRICAL_SURFACE('',#9305,0.3);
#8230=CYLINDRICAL_SURFACE('',#9310,0.3);
#8231=CYLINDRICAL_SURFACE('',#9315,0.14635);
#8232=CYLINDRICAL_SURFACE('',#9317,0.14635);
#8233=CYLINDRICAL_SURFACE('',#9318,0.14635);
#8234=CYLINDRICAL_SURFACE('',#9319,0.14635);
#8235=CYLINDRICAL_SURFACE('',#9320,0.14635);
#8236=CYLINDRICAL_SURFACE('',#9321,0.14635);
#8237=CYLINDRICAL_SURFACE('',#9322,0.14635);
#8238=CYLINDRICAL_SURFACE('',#9323,0.14635);
#8239=CYLINDRICAL_SURFACE('',#9324,0.14635);
#8240=CYLINDRICAL_SURFACE('',#9325,0.14635);
#8241=CYLINDRICAL_SURFACE('',#9326,0.14635);
#8242=CYLINDRICAL_SURFACE('',#9327,0.14635);
#8243=CYLINDRICAL_SURFACE('',#9328,0.14635);
#8244=CYLINDRICAL_SURFACE('',#9329,0.14635);
#8245=CYLINDRICAL_SURFACE('',#9330,0.14635);
#8246=CYLINDRICAL_SURFACE('',#9331,0.14635);
#8247=CYLINDRICAL_SURFACE('',#9332,0.14635);
#8248=CYLINDRICAL_SURFACE('',#9333,0.14635);
#8249=CYLINDRICAL_SURFACE('',#9334,0.14635);
#8250=CYLINDRICAL_SURFACE('',#9335,0.14635);
#8251=CYLINDRICAL_SURFACE('',#9336,0.14635);
#8252=CYLINDRICAL_SURFACE('',#9337,0.14635);
#8253=CYLINDRICAL_SURFACE('',#9338,0.14635);
#8254=CYLINDRICAL_SURFACE('',#9339,0.14635);
#8255=CYLINDRICAL_SURFACE('',#9340,0.14635);
#8256=CYLINDRICAL_SURFACE('',#9341,0.14635);
#8257=CYLINDRICAL_SURFACE('',#9342,0.14635);
#8258=CYLINDRICAL_SURFACE('',#9343,0.14635);
#8259=CYLINDRICAL_SURFACE('',#9344,0.14635);
#8260=CYLINDRICAL_SURFACE('',#9345,0.14635);
#8261=CYLINDRICAL_SURFACE('',#9346,0.117775);
#8262=CYLINDRICAL_SURFACE('',#9348,0.117775);
#8263=CYLINDRICAL_SURFACE('',#9349,0.117775);
#8264=CYLINDRICAL_SURFACE('',#9350,0.117775);
#8265=CYLINDRICAL_SURFACE('',#9351,0.117775);
#8266=CYLINDRICAL_SURFACE('',#9352,0.117775);
#8267=CYLINDRICAL_SURFACE('',#9353,0.117775);
#8268=CYLINDRICAL_SURFACE('',#9354,0.117775);
#8269=CYLINDRICAL_SURFACE('',#9355,0.117775);
#8270=CYLINDRICAL_SURFACE('',#9356,0.117775);
#8271=CYLINDRICAL_SURFACE('',#9357,0.117775);
#8272=CYLINDRICAL_SURFACE('',#9358,0.117775);
#8273=CYLINDRICAL_SURFACE('',#9359,0.117775);
#8274=CYLINDRICAL_SURFACE('',#9360,0.117775);
#8275=CYLINDRICAL_SURFACE('',#9361,0.117775);
#8276=CYLINDRICAL_SURFACE('',#9362,0.117775);
#8277=CYLINDRICAL_SURFACE('',#9363,0.117775);
#8278=CYLINDRICAL_SURFACE('',#9364,0.117775);
#8279=CYLINDRICAL_SURFACE('',#9365,0.117775);
#8280=CYLINDRICAL_SURFACE('',#9366,0.117775);
#8281=CYLINDRICAL_SURFACE('',#9367,0.117775);
#8282=CYLINDRICAL_SURFACE('',#9368,0.117775);
#8283=CYLINDRICAL_SURFACE('',#9369,0.117775);
#8284=CYLINDRICAL_SURFACE('',#9370,0.117775);
#8285=CYLINDRICAL_SURFACE('',#9371,0.117775);
#8286=CYLINDRICAL_SURFACE('',#9372,0.117775);
#8287=CYLINDRICAL_SURFACE('',#9373,0.117775);
#8288=CYLINDRICAL_SURFACE('',#9374,0.117775);
#8289=CYLINDRICAL_SURFACE('',#9375,0.117775);
#8290=CYLINDRICAL_SURFACE('',#9376,0.117775);
#8291=CYLINDRICAL_SURFACE('',#9380,0.117775);
#8292=CYLINDRICAL_SURFACE('',#9382,0.14635);
#8293=CYLINDRICAL_SURFACE('',#9392,0.275);
#8294=CYLINDRICAL_SURFACE('',#9397,0.12645);
#8295=CYLINDRICAL_SURFACE('',#9399,0.12645);
#8296=CYLINDRICAL_SURFACE('',#9401,0.12645);
#8297=CYLINDRICAL_SURFACE('',#9402,0.12645);
#8298=CYLINDRICAL_SURFACE('',#9403,0.12645);
#8299=CYLINDRICAL_SURFACE('',#9405,0.1543);
#8300=CYLINDRICAL_SURFACE('',#9407,0.1543);
#8301=CYLINDRICAL_SURFACE('',#9408,0.1543);
#8302=CYLINDRICAL_SURFACE('',#9409,0.1543);
#8303=CYLINDRICAL_SURFACE('',#9410,0.1543);
#8304=CYLINDRICAL_SURFACE('',#9412,0.1543);
#8305=CYLINDRICAL_SURFACE('',#9414,0.12645);
#8306=CYLINDRICAL_SURFACE('',#9423,0.35);
#8307=CYLINDRICAL_SURFACE('',#9426,0.35);
#8308=CYLINDRICAL_SURFACE('',#9432,0.25);
#8309=CYLINDRICAL_SURFACE('',#9438,0.25);
#8310=CYLINDRICAL_SURFACE('',#9444,0.25);
#8311=CYLINDRICAL_SURFACE('',#9450,0.25);
#8312=CYLINDRICAL_SURFACE('',#9453,0.15);
#8313=CYLINDRICAL_SURFACE('',#9455,0.15);
#8314=CYLINDRICAL_SURFACE('',#9457,0.15);
#8315=CYLINDRICAL_SURFACE('',#9459,0.15);
#8316=CYLINDRICAL_SURFACE('',#9463,0.08);
#8317=CYLINDRICAL_SURFACE('',#9468,0.08);
#8318=CYLINDRICAL_SURFACE('',#9484,0.41);
#8319=CYLINDRICAL_SURFACE('',#9487,0.6);
#8320=ADVANCED_FACE('',(#903),#8186,.F.);
#8321=ADVANCED_FACE('',(#904),#8187,.F.);
#8322=ADVANCED_FACE('',(#905),#8188,.F.);
#8323=ADVANCED_FACE('',(#906),#651,.F.);
#8324=ADVANCED_FACE('',(#907),#652,.F.);
#8325=ADVANCED_FACE('',(#908),#653,.F.);
#8326=ADVANCED_FACE('',(#909),#654,.F.);
#8327=ADVANCED_FACE('',(#910),#655,.F.);
#8328=ADVANCED_FACE('',(#911),#656,.F.);
#8329=ADVANCED_FACE('',(#912),#657,.F.);
#8330=ADVANCED_FACE('',(#913),#658,.F.);
#8331=ADVANCED_FACE('',(#914),#659,.F.);
#8332=ADVANCED_FACE('',(#915),#660,.F.);
#8333=ADVANCED_FACE('',(#916),#661,.F.);
#8334=ADVANCED_FACE('',(#917),#662,.F.);
#8335=ADVANCED_FACE('',(#918),#663,.F.);
#8336=ADVANCED_FACE('',(#919),#664,.F.);
#8337=ADVANCED_FACE('',(#920),#665,.F.);
#8338=ADVANCED_FACE('',(#921),#666,.F.);
#8339=ADVANCED_FACE('',(#922),#667,.F.);
#8340=ADVANCED_FACE('',(#923),#668,.F.);
#8341=ADVANCED_FACE('',(#924),#669,.F.);
#8342=ADVANCED_FACE('',(#925),#670,.F.);
#8343=ADVANCED_FACE('',(#926),#671,.F.);
#8344=ADVANCED_FACE('',(#927),#672,.F.);
#8345=ADVANCED_FACE('',(#928),#673,.F.);
#8346=ADVANCED_FACE('',(#929),#674,.F.);
#8347=ADVANCED_FACE('',(#930),#675,.F.);
#8348=ADVANCED_FACE('',(#931),#676,.F.);
#8349=ADVANCED_FACE('',(#932),#677,.F.);
#8350=ADVANCED_FACE('',(#933),#678,.F.);
#8351=ADVANCED_FACE('',(#934),#679,.F.);
#8352=ADVANCED_FACE('',(#935),#680,.F.);
#8353=ADVANCED_FACE('',(#936),#681,.F.);
#8354=ADVANCED_FACE('',(#937),#682,.F.);
#8355=ADVANCED_FACE('',(#938),#683,.F.);
#8356=ADVANCED_FACE('',(#939),#684,.F.);
#8357=ADVANCED_FACE('',(#940),#685,.F.);
#8358=ADVANCED_FACE('',(#941),#686,.F.);
#8359=ADVANCED_FACE('',(#942),#687,.F.);
#8360=ADVANCED_FACE('',(#943),#688,.F.);
#8361=ADVANCED_FACE('',(#944),#689,.F.);
#8362=ADVANCED_FACE('',(#945),#690,.F.);
#8363=ADVANCED_FACE('',(#946),#691,.F.);
#8364=ADVANCED_FACE('',(#947),#692,.F.);
#8365=ADVANCED_FACE('',(#948),#693,.F.);
#8366=ADVANCED_FACE('',(#949),#694,.F.);
#8367=ADVANCED_FACE('',(#950),#695,.F.);
#8368=ADVANCED_FACE('',(#951),#696,.F.);
#8369=ADVANCED_FACE('',(#952),#697,.F.);
#8370=ADVANCED_FACE('',(#953),#698,.F.);
#8371=ADVANCED_FACE('',(#954),#699,.F.);
#8372=ADVANCED_FACE('',(#955),#700,.F.);
#8373=ADVANCED_FACE('',(#956),#701,.F.);
#8374=ADVANCED_FACE('',(#957),#702,.F.);
#8375=ADVANCED_FACE('',(#958),#703,.F.);
#8376=ADVANCED_FACE('',(#959),#704,.F.);
#8377=ADVANCED_FACE('',(#960),#705,.F.);
#8378=ADVANCED_FACE('',(#961),#706,.F.);
#8379=ADVANCED_FACE('',(#962),#707,.F.);
#8380=ADVANCED_FACE('',(#963),#708,.F.);
#8381=ADVANCED_FACE('',(#964),#709,.F.);
#8382=ADVANCED_FACE('',(#965),#710,.F.);
#8383=ADVANCED_FACE('',(#966),#711,.F.);
#8384=ADVANCED_FACE('',(#967),#712,.F.);
#8385=ADVANCED_FACE('',(#968),#713,.F.);
#8386=ADVANCED_FACE('',(#969),#714,.F.);
#8387=ADVANCED_FACE('',(#970),#715,.F.);
#8388=ADVANCED_FACE('',(#971),#716,.F.);
#8389=ADVANCED_FACE('',(#972),#717,.F.);
#8390=ADVANCED_FACE('',(#973),#718,.F.);
#8391=ADVANCED_FACE('',(#974),#719,.F.);
#8392=ADVANCED_FACE('',(#975),#720,.F.);
#8393=ADVANCED_FACE('',(#976),#721,.F.);
#8394=ADVANCED_FACE('',(#977),#722,.F.);
#8395=ADVANCED_FACE('',(#978),#723,.F.);
#8396=ADVANCED_FACE('',(#979),#724,.F.);
#8397=ADVANCED_FACE('',(#980),#725,.F.);
#8398=ADVANCED_FACE('',(#981),#726,.F.);
#8399=ADVANCED_FACE('',(#982),#727,.T.);
#8400=ADVANCED_FACE('',(#983),#728,.T.);
#8401=ADVANCED_FACE('',(#984),#729,.T.);
#8402=ADVANCED_FACE('',(#985),#730,.T.);
#8403=ADVANCED_FACE('',(#986),#731,.T.);
#8404=ADVANCED_FACE('',(#987),#732,.T.);
#8405=ADVANCED_FACE('',(#988),#733,.T.);
#8406=ADVANCED_FACE('',(#989),#734,.T.);
#8407=ADVANCED_FACE('',(#990),#735,.T.);
#8408=ADVANCED_FACE('',(#991),#736,.T.);
#8409=ADVANCED_FACE('',(#992),#737,.T.);
#8410=ADVANCED_FACE('',(#993),#738,.T.);
#8411=ADVANCED_FACE('',(#994),#739,.T.);
#8412=ADVANCED_FACE('',(#995),#740,.T.);
#8413=ADVANCED_FACE('',(#996),#741,.T.);
#8414=ADVANCED_FACE('',(#997),#742,.T.);
#8415=ADVANCED_FACE('',(#998),#743,.T.);
#8416=ADVANCED_FACE('',(#999),#744,.T.);
#8417=ADVANCED_FACE('',(#1000),#745,.T.);
#8418=ADVANCED_FACE('',(#1001),#746,.T.);
#8419=ADVANCED_FACE('',(#1002),#747,.T.);
#8420=ADVANCED_FACE('',(#1003),#748,.T.);
#8421=ADVANCED_FACE('',(#1004),#749,.T.);
#8422=ADVANCED_FACE('',(#1005),#750,.T.);
#8423=ADVANCED_FACE('',(#1006),#751,.T.);
#8424=ADVANCED_FACE('',(#1007),#752,.T.);
#8425=ADVANCED_FACE('',(#1008),#753,.T.);
#8426=ADVANCED_FACE('',(#1009),#754,.T.);
#8427=ADVANCED_FACE('',(#1010),#755,.T.);
#8428=ADVANCED_FACE('',(#1011),#756,.T.);
#8429=ADVANCED_FACE('',(#1012),#757,.T.);
#8430=ADVANCED_FACE('',(#1013),#758,.T.);
#8431=ADVANCED_FACE('',(#1014),#759,.T.);
#8432=ADVANCED_FACE('',(#1015),#760,.T.);
#8433=ADVANCED_FACE('',(#1016),#761,.T.);
#8434=ADVANCED_FACE('',(#1017),#762,.T.);
#8435=ADVANCED_FACE('',(#1018),#763,.T.);
#8436=ADVANCED_FACE('',(#1019),#764,.T.);
#8437=ADVANCED_FACE('',(#1020),#765,.T.);
#8438=ADVANCED_FACE('',(#1021),#766,.F.);
#8439=ADVANCED_FACE('',(#1022),#767,.T.);
#8440=ADVANCED_FACE('',(#1023),#768,.T.);
#8441=ADVANCED_FACE('',(#1024),#769,.T.);
#8442=ADVANCED_FACE('',(#1025),#770,.T.);
#8443=ADVANCED_FACE('',(#1026),#771,.T.);
#8444=ADVANCED_FACE('',(#1027,#590,#591,#592),#772,.F.);
#8445=ADVANCED_FACE('',(#1028),#8189,.T.);
#8446=ADVANCED_FACE('',(#1029),#773,.T.);
#8447=ADVANCED_FACE('',(#1030),#774,.T.);
#8448=ADVANCED_FACE('',(#1031),#775,.T.);
#8449=ADVANCED_FACE('',(#1032),#776,.T.);
#8450=ADVANCED_FACE('',(#1033),#777,.T.);
#8451=ADVANCED_FACE('',(#1034),#778,.T.);
#8452=ADVANCED_FACE('',(#1035,#593,#594,#595),#779,.T.);
#8453=ADVANCED_FACE('',(#1036),#8190,.T.);
#8454=ADVANCED_FACE('',(#1037),#8191,.T.);
#8455=ADVANCED_FACE('',(#1038,#596),#780,.F.);
#8456=ADVANCED_FACE('',(#1039,#597),#781,.F.);
#8457=ADVANCED_FACE('',(#1040),#8192,.T.);
#8458=ADVANCED_FACE('',(#1041,#598),#782,.T.);
#8459=ADVANCED_FACE('',(#1042),#8193,.T.);
#8460=ADVANCED_FACE('',(#1043),#783,.F.);
#8461=ADVANCED_FACE('',(#1044),#8194,.T.);
#8462=ADVANCED_FACE('',(#1045),#784,.T.);
#8463=ADVANCED_FACE('',(#1046),#785,.F.);
#8464=ADVANCED_FACE('',(#1047),#786,.F.);
#8465=ADVANCED_FACE('',(#1048),#787,.F.);
#8466=ADVANCED_FACE('',(#1049),#8195,.F.);
#8467=ADVANCED_FACE('',(#1050),#8196,.T.);
#8468=ADVANCED_FACE('',(#1051),#788,.T.);
#8469=ADVANCED_FACE('',(#1052),#8197,.F.);
#8470=ADVANCED_FACE('',(#1053),#8198,.F.);
#8471=ADVANCED_FACE('',(#1054),#8199,.F.);
#8472=ADVANCED_FACE('',(#1055),#8200,.F.);
#8473=ADVANCED_FACE('',(#1056),#92,.T.);
#8474=ADVANCED_FACE('',(#1057),#93,.T.);
#8475=ADVANCED_FACE('',(#1058,#599,#600,#601),#789,.F.);
#8476=ADVANCED_FACE('',(#1059),#8201,.F.);
#8477=ADVANCED_FACE('',(#1060),#8202,.F.);
#8478=ADVANCED_FACE('',(#1061),#8203,.F.);
#8479=ADVANCED_FACE('',(#1062),#8204,.F.);
#8480=ADVANCED_FACE('',(#1063),#8205,.F.);
#8481=ADVANCED_FACE('',(#1064,#602),#790,.F.);
#8482=ADVANCED_FACE('',(#1065),#8206,.F.);
#8483=ADVANCED_FACE('',(#1066,#603),#791,.F.);
#8484=ADVANCED_FACE('',(#1067),#8207,.F.);
#8485=ADVANCED_FACE('',(#1068),#8208,.F.);
#8486=ADVANCED_FACE('',(#1069),#792,.F.);
#8487=ADVANCED_FACE('',(#1070),#793,.F.);
#8488=ADVANCED_FACE('',(#1071),#794,.F.);
#8489=ADVANCED_FACE('',(#1072),#795,.F.);
#8490=ADVANCED_FACE('',(#1073),#796,.F.);
#8491=ADVANCED_FACE('',(#1074),#797,.F.);
#8492=ADVANCED_FACE('',(#1075),#798,.F.);
#8493=ADVANCED_FACE('',(#1076,#604),#799,.F.);
#8494=ADVANCED_FACE('',(#1077,#605),#800,.F.);
#8495=ADVANCED_FACE('',(#1078),#801,.F.);
#8496=ADVANCED_FACE('',(#1079),#802,.F.);
#8497=ADVANCED_FACE('',(#1080),#803,.F.);
#8498=ADVANCED_FACE('',(#1081),#804,.F.);
#8499=ADVANCED_FACE('',(#1082),#805,.F.);
#8500=ADVANCED_FACE('',(#1083),#806,.T.);
#8501=ADVANCED_FACE('',(#1084),#807,.T.);
#8502=ADVANCED_FACE('',(#1085),#808,.T.);
#8503=ADVANCED_FACE('',(#1086),#809,.T.);
#8504=ADVANCED_FACE('',(#1087),#810,.T.);
#8505=ADVANCED_FACE('',(#1088,#606),#811,.F.);
#8506=ADVANCED_FACE('',(#1089),#8209,.T.);
#8507=ADVANCED_FACE('',(#1090),#8210,.T.);
#8508=ADVANCED_FACE('',(#1091),#812,.T.);
#8509=ADVANCED_FACE('',(#1092),#94,.T.);
#8510=ADVANCED_FACE('',(#1093),#95,.T.);
#8511=ADVANCED_FACE('',(#1094),#96,.T.);
#8512=ADVANCED_FACE('',(#1095),#97,.T.);
#8513=ADVANCED_FACE('',(#1096),#813,.F.);
#8514=ADVANCED_FACE('',(#1097),#98,.T.);
#8515=ADVANCED_FACE('',(#1098),#99,.T.);
#8516=ADVANCED_FACE('',(#1099),#814,.T.);
#8517=ADVANCED_FACE('',(#1100),#100,.T.);
#8518=ADVANCED_FACE('',(#1101),#101,.T.);
#8519=ADVANCED_FACE('',(#1102),#815,.F.);
#8520=ADVANCED_FACE('',(#1103),#102,.T.);
#8521=ADVANCED_FACE('',(#1104),#103,.T.);
#8522=ADVANCED_FACE('',(#1105),#816,.T.);
#8523=ADVANCED_FACE('',(#1106),#104,.T.);
#8524=ADVANCED_FACE('',(#1107),#105,.T.);
#8525=ADVANCED_FACE('',(#1108,#607,#608,#609),#817,.F.);
#8526=ADVANCED_FACE('',(#1109),#106,.T.);
#8527=ADVANCED_FACE('',(#1110),#818,.T.);
#8528=ADVANCED_FACE('',(#1111),#107,.T.);
#8529=ADVANCED_FACE('',(#1112),#108,.T.);
#8530=ADVANCED_FACE('',(#1113),#819,.F.);
#8531=ADVANCED_FACE('',(#1114),#109,.T.);
#8532=ADVANCED_FACE('',(#1115),#110,.T.);
#8533=ADVANCED_FACE('',(#1116),#76,.F.);
#8534=ADVANCED_FACE('',(#1117),#77,.F.);
#8535=ADVANCED_FACE('',(#1118),#78,.F.);
#8536=ADVANCED_FACE('',(#1119),#8211,.F.);
#8537=ADVANCED_FACE('',(#1120),#111,.T.);
#8538=ADVANCED_FACE('',(#1121),#79,.F.);
#8539=ADVANCED_FACE('',(#1122),#8212,.F.);
#8540=ADVANCED_FACE('',(#1123),#112,.T.);
#8541=ADVANCED_FACE('',(#1124),#113,.T.);
#8542=ADVANCED_FACE('',(#1125),#114,.T.);
#8543=ADVANCED_FACE('',(#1126),#115,.T.);
#8544=ADVANCED_FACE('',(#1127),#820,.T.);
#8545=ADVANCED_FACE('',(#1128),#80,.T.);
#8546=ADVANCED_FACE('',(#1129),#81,.T.);
#8547=ADVANCED_FACE('',(#1130),#82,.T.);
#8548=ADVANCED_FACE('',(#1131),#8213,.T.);
#8549=ADVANCED_FACE('',(#1132),#116,.F.);
#8550=ADVANCED_FACE('',(#1133),#83,.T.);
#8551=ADVANCED_FACE('',(#1134),#8214,.T.);
#8552=ADVANCED_FACE('',(#1135),#117,.F.);
#8553=ADVANCED_FACE('',(#1136),#118,.F.);
#8554=ADVANCED_FACE('',(#1137),#119,.F.);
#8555=ADVANCED_FACE('',(#1138),#120,.F.);
#8556=ADVANCED_FACE('',(#1139),#121,.F.);
#8557=ADVANCED_FACE('',(#1140),#122,.F.);
#8558=ADVANCED_FACE('',(#1141),#821,.F.);
#8559=ADVANCED_FACE('',(#1142,#610,#611,#612,#613,#614,#615),#822,.T.);
#8560=ADVANCED_FACE('',(#1143),#123,.F.);
#8561=ADVANCED_FACE('',(#1144),#823,.F.);
#8562=ADVANCED_FACE('',(#1145),#8215,.F.);
#8563=ADVANCED_FACE('',(#1146),#8216,.F.);
#8564=ADVANCED_FACE('',(#1147),#8217,.F.);
#8565=ADVANCED_FACE('',(#1148),#8218,.F.);
#8566=ADVANCED_FACE('',(#1149),#124,.T.);
#8567=ADVANCED_FACE('',(#1150),#125,.T.);
#8568=ADVANCED_FACE('',(#1151,#616,#617,#618),#824,.F.);
#8569=ADVANCED_FACE('',(#1152),#825,.F.);
#8570=ADVANCED_FACE('',(#1153),#826,.F.);
#8571=ADVANCED_FACE('',(#1154),#827,.F.);
#8572=ADVANCED_FACE('',(#1155),#828,.F.);
#8573=ADVANCED_FACE('',(#1156),#829,.F.);
#8574=ADVANCED_FACE('',(#1157),#830,.F.);
#8575=ADVANCED_FACE('',(#1158,#619),#831,.F.);
#8576=ADVANCED_FACE('',(#1159),#832,.F.);
#8577=ADVANCED_FACE('',(#1160),#833,.F.);
#8578=ADVANCED_FACE('',(#1161),#834,.F.);
#8579=ADVANCED_FACE('',(#1162),#835,.F.);
#8580=ADVANCED_FACE('',(#1163),#836,.F.);
#8581=ADVANCED_FACE('',(#1164),#837,.F.);
#8582=ADVANCED_FACE('',(#1165,#620),#838,.F.);
#8583=ADVANCED_FACE('',(#1166),#8219,.F.);
#8584=ADVANCED_FACE('',(#1167),#8220,.F.);
#8585=ADVANCED_FACE('',(#1168),#8221,.F.);
#8586=ADVANCED_FACE('',(#1169),#8222,.F.);
#8587=ADVANCED_FACE('',(#1170),#8223,.F.);
#8588=ADVANCED_FACE('',(#1171),#8224,.F.);
#8589=ADVANCED_FACE('',(#1172),#839,.F.);
#8590=ADVANCED_FACE('',(#1173),#840,.F.);
#8591=ADVANCED_FACE('',(#1174),#841,.F.);
#8592=ADVANCED_FACE('',(#1175),#842,.F.);
#8593=ADVANCED_FACE('',(#1176),#843,.F.);
#8594=ADVANCED_FACE('',(#1177),#844,.F.);
#8595=ADVANCED_FACE('',(#1178),#845,.F.);
#8596=ADVANCED_FACE('',(#1179,#621),#846,.F.);
#8597=ADVANCED_FACE('',(#1180,#622),#847,.F.);
#8598=ADVANCED_FACE('',(#1181),#848,.F.);
#8599=ADVANCED_FACE('',(#1182),#849,.F.);
#8600=ADVANCED_FACE('',(#1183),#850,.F.);
#8601=ADVANCED_FACE('',(#1184),#851,.F.);
#8602=ADVANCED_FACE('',(#1185),#852,.F.);
#8603=ADVANCED_FACE('',(#1186),#853,.T.);
#8604=ADVANCED_FACE('',(#1187),#854,.T.);
#8605=ADVANCED_FACE('',(#1188),#855,.T.);
#8606=ADVANCED_FACE('',(#1189),#856,.T.);
#8607=ADVANCED_FACE('',(#1190),#857,.T.);
#8608=ADVANCED_FACE('',(#1191,#623),#858,.F.);
#8609=ADVANCED_FACE('',(#1192),#8225,.T.);
#8610=ADVANCED_FACE('',(#1193),#8226,.T.);
#8611=ADVANCED_FACE('',(#1194),#859,.T.);
#8612=ADVANCED_FACE('',(#1195),#126,.T.);
#8613=ADVANCED_FACE('',(#1196),#127,.T.);
#8614=ADVANCED_FACE('',(#1197),#128,.T.);
#8615=ADVANCED_FACE('',(#1198),#129,.T.);
#8616=ADVANCED_FACE('',(#1199),#860,.F.);
#8617=ADVANCED_FACE('',(#1200),#130,.T.);
#8618=ADVANCED_FACE('',(#1201),#131,.T.);
#8619=ADVANCED_FACE('',(#1202),#861,.T.);
#8620=ADVANCED_FACE('',(#1203),#132,.T.);
#8621=ADVANCED_FACE('',(#1204),#133,.T.);
#8622=ADVANCED_FACE('',(#1205),#862,.F.);
#8623=ADVANCED_FACE('',(#1206),#134,.T.);
#8624=ADVANCED_FACE('',(#1207),#135,.T.);
#8625=ADVANCED_FACE('',(#1208),#863,.T.);
#8626=ADVANCED_FACE('',(#1209),#136,.T.);
#8627=ADVANCED_FACE('',(#1210),#137,.T.);
#8628=ADVANCED_FACE('',(#1211,#624,#625,#626),#864,.F.);
#8629=ADVANCED_FACE('',(#1212),#138,.T.);
#8630=ADVANCED_FACE('',(#1213),#865,.T.);
#8631=ADVANCED_FACE('',(#1214),#139,.T.);
#8632=ADVANCED_FACE('',(#1215),#140,.T.);
#8633=ADVANCED_FACE('',(#1216),#866,.F.);
#8634=ADVANCED_FACE('',(#1217),#141,.T.);
#8635=ADVANCED_FACE('',(#1218),#142,.T.);
#8636=ADVANCED_FACE('',(#1219),#84,.F.);
#8637=ADVANCED_FACE('',(#1220),#85,.F.);
#8638=ADVANCED_FACE('',(#1221),#86,.F.);
#8639=ADVANCED_FACE('',(#1222),#8227,.F.);
#8640=ADVANCED_FACE('',(#1223),#143,.T.);
#8641=ADVANCED_FACE('',(#1224),#87,.F.);
#8642=ADVANCED_FACE('',(#1225),#8228,.F.);
#8643=ADVANCED_FACE('',(#1226),#144,.T.);
#8644=ADVANCED_FACE('',(#1227),#145,.T.);
#8645=ADVANCED_FACE('',(#1228),#146,.T.);
#8646=ADVANCED_FACE('',(#1229),#147,.T.);
#8647=ADVANCED_FACE('',(#1230),#867,.T.);
#8648=ADVANCED_FACE('',(#1231),#88,.T.);
#8649=ADVANCED_FACE('',(#1232),#89,.T.);
#8650=ADVANCED_FACE('',(#1233),#90,.T.);
#8651=ADVANCED_FACE('',(#1234),#8229,.T.);
#8652=ADVANCED_FACE('',(#1235),#148,.F.);
#8653=ADVANCED_FACE('',(#1236),#91,.T.);
#8654=ADVANCED_FACE('',(#1237),#8230,.T.);
#8655=ADVANCED_FACE('',(#1238),#149,.F.);
#8656=ADVANCED_FACE('',(#1239),#150,.F.);
#8657=ADVANCED_FACE('',(#1240),#151,.F.);
#8658=ADVANCED_FACE('',(#1241),#152,.F.);
#8659=ADVANCED_FACE('',(#1242),#153,.F.);
#8660=ADVANCED_FACE('',(#1243),#154,.F.);
#8661=ADVANCED_FACE('',(#1244),#868,.F.);
#8662=ADVANCED_FACE('',(#1245,#627,#628,#629,#630,#631,#632),#869,.T.);
#8663=ADVANCED_FACE('',(#1246),#155,.F.);
#8664=ADVANCED_FACE('',(#1247),#870,.F.);
#8665=ADVANCED_FACE('',(#1248),#8231,.T.);
#8666=ADVANCED_FACE('',(#1249),#8232,.T.);
#8667=ADVANCED_FACE('',(#1250),#8233,.T.);
#8668=ADVANCED_FACE('',(#1251),#8234,.T.);
#8669=ADVANCED_FACE('',(#1252),#8235,.T.);
#8670=ADVANCED_FACE('',(#1253),#8236,.T.);
#8671=ADVANCED_FACE('',(#1254),#8237,.T.);
#8672=ADVANCED_FACE('',(#1255),#8238,.T.);
#8673=ADVANCED_FACE('',(#1256),#8239,.T.);
#8674=ADVANCED_FACE('',(#1257),#8240,.T.);
#8675=ADVANCED_FACE('',(#1258),#8241,.T.);
#8676=ADVANCED_FACE('',(#1259),#8242,.T.);
#8677=ADVANCED_FACE('',(#1260),#8243,.T.);
#8678=ADVANCED_FACE('',(#1261),#8244,.T.);
#8679=ADVANCED_FACE('',(#1262),#8245,.T.);
#8680=ADVANCED_FACE('',(#1263),#8246,.T.);
#8681=ADVANCED_FACE('',(#1264),#8247,.T.);
#8682=ADVANCED_FACE('',(#1265),#8248,.T.);
#8683=ADVANCED_FACE('',(#1266),#8249,.T.);
#8684=ADVANCED_FACE('',(#1267),#8250,.T.);
#8685=ADVANCED_FACE('',(#1268),#8251,.T.);
#8686=ADVANCED_FACE('',(#1269),#8252,.T.);
#8687=ADVANCED_FACE('',(#1270),#8253,.T.);
#8688=ADVANCED_FACE('',(#1271),#8254,.T.);
#8689=ADVANCED_FACE('',(#1272),#8255,.T.);
#8690=ADVANCED_FACE('',(#1273),#8256,.T.);
#8691=ADVANCED_FACE('',(#1274),#8257,.T.);
#8692=ADVANCED_FACE('',(#1275),#8258,.T.);
#8693=ADVANCED_FACE('',(#1276),#8259,.T.);
#8694=ADVANCED_FACE('',(#1277),#8260,.T.);
#8695=ADVANCED_FACE('',(#1278),#8261,.T.);
#8696=ADVANCED_FACE('',(#1279),#8262,.T.);
#8697=ADVANCED_FACE('',(#1280),#8263,.T.);
#8698=ADVANCED_FACE('',(#1281),#8264,.T.);
#8699=ADVANCED_FACE('',(#1282),#8265,.T.);
#8700=ADVANCED_FACE('',(#1283),#8266,.T.);
#8701=ADVANCED_FACE('',(#1284),#8267,.T.);
#8702=ADVANCED_FACE('',(#1285),#8268,.T.);
#8703=ADVANCED_FACE('',(#1286),#8269,.T.);
#8704=ADVANCED_FACE('',(#1287),#8270,.T.);
#8705=ADVANCED_FACE('',(#1288),#8271,.T.);
#8706=ADVANCED_FACE('',(#1289),#8272,.T.);
#8707=ADVANCED_FACE('',(#1290),#8273,.T.);
#8708=ADVANCED_FACE('',(#1291),#8274,.T.);
#8709=ADVANCED_FACE('',(#1292),#8275,.T.);
#8710=ADVANCED_FACE('',(#1293),#8276,.T.);
#8711=ADVANCED_FACE('',(#1294),#8277,.T.);
#8712=ADVANCED_FACE('',(#1295),#8278,.T.);
#8713=ADVANCED_FACE('',(#1296),#8279,.T.);
#8714=ADVANCED_FACE('',(#1297),#8280,.T.);
#8715=ADVANCED_FACE('',(#1298),#8281,.T.);
#8716=ADVANCED_FACE('',(#1299),#8282,.T.);
#8717=ADVANCED_FACE('',(#1300),#8283,.T.);
#8718=ADVANCED_FACE('',(#1301),#8284,.T.);
#8719=ADVANCED_FACE('',(#1302),#8285,.T.);
#8720=ADVANCED_FACE('',(#1303),#8286,.T.);
#8721=ADVANCED_FACE('',(#1304),#8287,.T.);
#8722=ADVANCED_FACE('',(#1305),#8288,.T.);
#8723=ADVANCED_FACE('',(#1306),#8289,.T.);
#8724=ADVANCED_FACE('',(#1307),#8290,.T.);
#8725=ADVANCED_FACE('',(#1308),#75,.T.);
#8726=ADVANCED_FACE('',(#1309),#156,.F.);
#8727=ADVANCED_FACE('',(#1310),#8291,.T.);
#8728=ADVANCED_FACE('',(#1311),#157,.F.);
#8729=ADVANCED_FACE('',(#1312),#8292,.T.);
#8730=ADVANCED_FACE('',(#1313),#871,.F.);
#8731=ADVANCED_FACE('',(#1314),#872,.F.);
#8732=ADVANCED_FACE('',(#1315),#873,.F.);
#8733=ADVANCED_FACE('',(#1316),#874,.F.);
#8734=ADVANCED_FACE('',(#1317),#875,.F.);
#8735=ADVANCED_FACE('',(#1318),#876,.F.);
#8736=ADVANCED_FACE('',(#1319),#877,.F.);
#8737=ADVANCED_FACE('',(#1320,#633),#878,.T.);
#8738=ADVANCED_FACE('',(#1321),#8293,.T.);
#8739=ADVANCED_FACE('',(#1322,#634),#879,.F.);
#8740=ADVANCED_FACE('',(#1323),#880,.T.);
#8741=ADVANCED_FACE('',(#1324),#8294,.F.);
#8742=ADVANCED_FACE('',(#1325),#8295,.F.);
#8743=ADVANCED_FACE('',(#1326),#8296,.F.);
#8744=ADVANCED_FACE('',(#1327),#8297,.F.);
#8745=ADVANCED_FACE('',(#1328),#8298,.F.);
#8746=ADVANCED_FACE('',(#1329),#8299,.F.);
#8747=ADVANCED_FACE('',(#1330),#8300,.F.);
#8748=ADVANCED_FACE('',(#1331),#8301,.F.);
#8749=ADVANCED_FACE('',(#1332),#8302,.F.);
#8750=ADVANCED_FACE('',(#1333),#8303,.F.);
#8751=ADVANCED_FACE('',(#1334),#8304,.F.);
#8752=ADVANCED_FACE('',(#1335),#158,.F.);
#8753=ADVANCED_FACE('',(#1336),#159,.F.);
#8754=ADVANCED_FACE('',(#1337,#635),#881,.T.);
#8755=ADVANCED_FACE('',(#1338),#8305,.F.);
#8756=ADVANCED_FACE('',(#1339),#882,.T.);
#8757=ADVANCED_FACE('',(#1340),#883,.T.);
#8758=ADVANCED_FACE('',(#1341),#884,.T.);
#8759=ADVANCED_FACE('',(#1342),#885,.T.);
#8760=ADVANCED_FACE('',(#1343),#886,.T.);
#8761=ADVANCED_FACE('',(#1344),#887,.T.);
#8762=ADVANCED_FACE('',(#1345,#636),#888,.F.);
#8763=ADVANCED_FACE('',(#1346),#8306,.F.);
#8764=ADVANCED_FACE('',(#1347),#8307,.F.);
#8765=ADVANCED_FACE('',(#1348,#637),#889,.T.);
#8766=ADVANCED_FACE('',(#1349),#8308,.T.);
#8767=ADVANCED_FACE('',(#1350),#890,.F.);
#8768=ADVANCED_FACE('',(#1351,#638),#891,.T.);
#8769=ADVANCED_FACE('',(#1352),#8309,.T.);
#8770=ADVANCED_FACE('',(#1353),#892,.F.);
#8771=ADVANCED_FACE('',(#1354,#639),#893,.T.);
#8772=ADVANCED_FACE('',(#1355),#8310,.T.);
#8773=ADVANCED_FACE('',(#1356),#894,.F.);
#8774=ADVANCED_FACE('',(#1357,#640),#895,.T.);
#8775=ADVANCED_FACE('',(#1358),#8311,.T.);
#8776=ADVANCED_FACE('',(#1359),#896,.F.);
#8777=ADVANCED_FACE('',(#1360),#8312,.T.);
#8778=ADVANCED_FACE('',(#1361),#8313,.T.);
#8779=ADVANCED_FACE('',(#1362),#8314,.T.);
#8780=ADVANCED_FACE('',(#1363),#8315,.T.);
#8781=ADVANCED_FACE('',(#1364),#160,.F.);
#8782=ADVANCED_FACE('',(#1365),#8316,.T.);
#8783=ADVANCED_FACE('',(#1366),#161,.F.);
#8784=ADVANCED_FACE('',(#1367),#162,.F.);
#8785=ADVANCED_FACE('',(#1368),#163,.F.);
#8786=ADVANCED_FACE('',(#1369),#8317,.T.);
#8787=ADVANCED_FACE('',(#1370),#164,.F.);
#8788=ADVANCED_FACE('',(#1371),#165,.F.);
#8789=ADVANCED_FACE('',(#1372),#897,.F.);
#8790=ADVANCED_FACE('',(#1373),#166,.F.);
#8791=ADVANCED_FACE('',(#1374),#167,.F.);
#8792=ADVANCED_FACE('',(#1375),#168,.F.);
#8793=ADVANCED_FACE('',(#1376,#641,#642),#898,.T.);
#8794=ADVANCED_FACE('',(#1377),#899,.F.);
#8795=ADVANCED_FACE('',(#1378),#169,.F.);
#8796=ADVANCED_FACE('',(#1379),#170,.F.);
#8797=ADVANCED_FACE('',(#1380,#643,#644,#645,#646,#647,#648),#900,.F.);
#8798=ADVANCED_FACE('',(#1381),#171,.F.);
#8799=ADVANCED_FACE('',(#1382),#8318,.F.);
#8800=ADVANCED_FACE('',(#1383),#8319,.T.);
#8801=ADVANCED_FACE('',(#1384,#649),#901,.T.);
#8802=ADVANCED_FACE('',(#1385,#650),#902,.F.);
#8803=CLOSED_SHELL('',(#8320,#8321,#8322,#8323,#8324,#8325,#8326,#8327,
#8328,#8329,#8330,#8331,#8332,#8333,#8334,#8335,#8336,#8337,#8338,#8339,
#8340,#8341,#8342,#8343,#8344,#8345,#8346,#8347,#8348,#8349,#8350,#8351,
#8352,#8353,#8354,#8355,#8356,#8357,#8358,#8359,#8360,#8361,#8362,#8363,
#8364,#8365,#8366,#8367,#8368,#8369,#8370,#8371,#8372,#8373,#8374,#8375,
#8376,#8377,#8378,#8379,#8380,#8381,#8382,#8383,#8384,#8385,#8386,#8387,
#8388,#8389,#8390,#8391,#8392,#8393,#8394,#8395,#8396,#8397,#8398,#8399,
#8400,#8401,#8402,#8403,#8404,#8405,#8406,#8407,#8408,#8409,#8410,#8411,
#8412,#8413,#8414,#8415,#8416,#8417,#8418,#8419,#8420,#8421,#8422,#8423,
#8424,#8425,#8426,#8427,#8428,#8429,#8430,#8431,#8432,#8433,#8434,#8435,
#8436,#8437,#8438,#8439,#8440,#8441,#8442,#8443,#8444,#8445,#8446,#8447,
#8448,#8449,#8450,#8451,#8452,#8453));
#8804=CLOSED_SHELL('',(#8454,#8455,#8456,#8457,#8458,#8459,#8460,#8461,
#8462));
#8805=CLOSED_SHELL('',(#8463,#8464,#8465,#8466,#8467,#8468));
#8806=CLOSED_SHELL('',(#8469,#8470,#8471,#8472,#8473,#8474,#8475,#8476,
#8477,#8478,#8479,#8480,#8481,#8482,#8483,#8484,#8485,#8486,#8487,#8488,
#8489,#8490,#8491,#8492,#8493,#8494,#8495,#8496,#8497,#8498,#8499,#8500,
#8501,#8502,#8503,#8504,#8505,#8506,#8507,#8508,#8509,#8510,#8511,#8512,
#8513,#8514,#8515,#8516,#8517,#8518,#8519,#8520,#8521,#8522,#8523,#8524,
#8525,#8526,#8527,#8528,#8529,#8530,#8531,#8532,#8533,#8534,#8535,#8536,
#8537,#8538,#8539,#8540,#8541,#8542,#8543,#8544,#8545,#8546,#8547,#8548,
#8549,#8550,#8551,#8552,#8553,#8554,#8555,#8556,#8557,#8558,#8559,#8560,
#8561));
#8807=CLOSED_SHELL('',(#8562,#8563,#8564,#8565,#8566,#8567,#8568,#8569,
#8570,#8571,#8572,#8573,#8574,#8575,#8576,#8577,#8578,#8579,#8580,#8581,
#8582,#8583,#8584,#8585,#8586,#8587,#8588,#8589,#8590,#8591,#8592,#8593,
#8594,#8595,#8596,#8597,#8598,#8599,#8600,#8601,#8602,#8603,#8604,#8605,
#8606,#8607,#8608,#8609,#8610,#8611,#8612,#8613,#8614,#8615,#8616,#8617,
#8618,#8619,#8620,#8621,#8622,#8623,#8624,#8625,#8626,#8627,#8628,#8629,
#8630,#8631,#8632,#8633,#8634,#8635,#8636,#8637,#8638,#8639,#8640,#8641,
#8642,#8643,#8644,#8645,#8646,#8647,#8648,#8649,#8650,#8651,#8652,#8653,
#8654,#8655,#8656,#8657,#8658,#8659,#8660,#8661,#8662,#8663,#8664));
#8808=CLOSED_SHELL('',(#8665,#8666,#8667,#8668,#8669,#8670,#8671,#8672,
#8673,#8674,#8675,#8676,#8677,#8678,#8679,#8680,#8681,#8682,#8683,#8684,
#8685,#8686,#8687,#8688,#8689,#8690,#8691,#8692,#8693,#8694,#8695,#8696,
#8697,#8698,#8699,#8700,#8701,#8702,#8703,#8704,#8705,#8706,#8707,#8708,
#8709,#8710,#8711,#8712,#8713,#8714,#8715,#8716,#8717,#8718,#8719,#8720,
#8721,#8722,#8723,#8724,#8725,#8726,#8727,#8728,#8729,#8730,#8731,#8732,
#8733,#8734,#8735,#8736,#8737,#8738,#8739,#8740));
#8809=CLOSED_SHELL('',(#8741,#8742,#8743,#8744,#8745,#8746,#8747,#8748,
#8749,#8750,#8751,#8752,#8753,#8754,#8755,#8756,#8757,#8758,#8759,#8760,
#8761,#8762));
#8810=CLOSED_SHELL('',(#8763,#8764,#8765,#8766,#8767,#8768,#8769,#8770,
#8771,#8772,#8773,#8774,#8775,#8776,#8777,#8778,#8779,#8780,#8781,#8782,
#8783,#8784,#8785,#8786,#8787,#8788,#8789,#8790,#8791,#8792,#8793,#8794,
#8795,#8796,#8797,#8798));
#8811=CLOSED_SHELL('',(#8799,#8800,#8801,#8802));
#8812=DERIVED_UNIT_ELEMENT(#8830,1.);
#8813=DERIVED_UNIT_ELEMENT(#22131,-3.);
#8814=DERIVED_UNIT_ELEMENT(#8830,1.);
#8815=DERIVED_UNIT_ELEMENT(#22131,-3.);
#8816=DERIVED_UNIT_ELEMENT(#8830,1.);
#8817=DERIVED_UNIT_ELEMENT(#22131,-3.);
#8818=DERIVED_UNIT_ELEMENT(#8830,1.);
#8819=DERIVED_UNIT_ELEMENT(#22131,-3.);
#8820=DERIVED_UNIT_ELEMENT(#8830,1.);
#8821=DERIVED_UNIT_ELEMENT(#22131,-3.);
#8822=DERIVED_UNIT_ELEMENT(#8830,1.);
#8823=DERIVED_UNIT_ELEMENT(#22131,-3.);
#8824=DERIVED_UNIT_ELEMENT(#8830,1.);
#8825=DERIVED_UNIT_ELEMENT(#22131,-3.);
#8826=DERIVED_UNIT_ELEMENT(#8830,1.);
#8827=DERIVED_UNIT_ELEMENT(#22131,-3.);
#8828=DERIVED_UNIT_ELEMENT(#8830,1.);
#8829=DERIVED_UNIT_ELEMENT(#22131,-3.);
#8830=(
MASS_UNIT()
NAMED_UNIT(*)
SI_UNIT(.KILO.,.GRAM.)
);
#8831=DERIVED_UNIT((#8812,#8813));
#8832=DERIVED_UNIT((#8814,#8815));
#8833=DERIVED_UNIT((#8816,#8817));
#8834=DERIVED_UNIT((#8818,#8819));
#8835=DERIVED_UNIT((#8820,#8821));
#8836=DERIVED_UNIT((#8822,#8823));
#8837=DERIVED_UNIT((#8824,#8825));
#8838=DERIVED_UNIT((#8826,#8827));
#8839=DERIVED_UNIT((#8828,#8829));
#8840=MEASURE_REPRESENTATION_ITEM('density measure',
POSITIVE_RATIO_MEASURE(7850.),#8831);
#8841=MEASURE_REPRESENTATION_ITEM('density measure',
POSITIVE_RATIO_MEASURE(7850.),#8832);
#8842=MEASURE_REPRESENTATION_ITEM('density measure',
POSITIVE_RATIO_MEASURE(7850.),#8833);
#8843=MEASURE_REPRESENTATION_ITEM('density measure',
POSITIVE_RATIO_MEASURE(7850.),#8834);
#8844=MEASURE_REPRESENTATION_ITEM('density measure',
POSITIVE_RATIO_MEASURE(7850.),#8835);
#8845=MEASURE_REPRESENTATION_ITEM('density measure',
POSITIVE_RATIO_MEASURE(7850.),#8836);
#8846=MEASURE_REPRESENTATION_ITEM('density measure',
POSITIVE_RATIO_MEASURE(7850.),#8837);
#8847=MEASURE_REPRESENTATION_ITEM('density measure',
POSITIVE_RATIO_MEASURE(7850.),#8838);
#8848=MEASURE_REPRESENTATION_ITEM('density measure',
POSITIVE_RATIO_MEASURE(7850.),#8839);
#8849=PROPERTY_DEFINITION_REPRESENTATION(#8894,#8867);
#8850=PROPERTY_DEFINITION_REPRESENTATION(#8895,#8868);
#8851=PROPERTY_DEFINITION_REPRESENTATION(#8896,#8869);
#8852=PROPERTY_DEFINITION_REPRESENTATION(#8897,#8870);
#8853=PROPERTY_DEFINITION_REPRESENTATION(#8898,#8871);
#8854=PROPERTY_DEFINITION_REPRESENTATION(#8899,#8872);
#8855=PROPERTY_DEFINITION_REPRESENTATION(#8900,#8873);
#8856=PROPERTY_DEFINITION_REPRESENTATION(#8901,#8874);
#8857=PROPERTY_DEFINITION_REPRESENTATION(#8902,#8875);
#8858=PROPERTY_DEFINITION_REPRESENTATION(#8903,#8876);
#8859=PROPERTY_DEFINITION_REPRESENTATION(#8904,#8877);
#8860=PROPERTY_DEFINITION_REPRESENTATION(#8905,#8878);
#8861=PROPERTY_DEFINITION_REPRESENTATION(#8906,#8879);
#8862=PROPERTY_DEFINITION_REPRESENTATION(#8907,#8880);
#8863=PROPERTY_DEFINITION_REPRESENTATION(#8908,#8881);
#8864=PROPERTY_DEFINITION_REPRESENTATION(#8909,#8882);
#8865=PROPERTY_DEFINITION_REPRESENTATION(#8910,#8883);
#8866=PROPERTY_DEFINITION_REPRESENTATION(#8911,#8884);
#8867=REPRESENTATION('material name',(#8885),#22119);
#8868=REPRESENTATION('density',(#8840),#22119);
#8869=REPRESENTATION('material name',(#8886),#22120);
#8870=REPRESENTATION('density',(#8841),#22120);
#8871=REPRESENTATION('material name',(#8887),#22121);
#8872=REPRESENTATION('density',(#8842),#22121);
#8873=REPRESENTATION('material name',(#8888),#22123);
#8874=REPRESENTATION('density',(#8843),#22123);
#8875=REPRESENTATION('material name',(#8889),#22124);
#8876=REPRESENTATION('density',(#8844),#22124);
#8877=REPRESENTATION('material name',(#8890),#22125);
#8878=REPRESENTATION('density',(#8845),#22125);
#8879=REPRESENTATION('material name',(#8891),#22126);
#8880=REPRESENTATION('density',(#8846),#22126);
#8881=REPRESENTATION('material name',(#8892),#22127);
#8882=REPRESENTATION('density',(#8847),#22127);
#8883=REPRESENTATION('material name',(#8893),#22128);
#8884=REPRESENTATION('density',(#8848),#22128);
#8885=DESCRIPTIVE_REPRESENTATION_ITEM('Steel','Steel');
#8886=DESCRIPTIVE_REPRESENTATION_ITEM('Steel','Steel');
#8887=DESCRIPTIVE_REPRESENTATION_ITEM('Steel','Steel');
#8888=DESCRIPTIVE_REPRESENTATION_ITEM('Steel','Steel');
#8889=DESCRIPTIVE_REPRESENTATION_ITEM('Steel','Steel');
#8890=DESCRIPTIVE_REPRESENTATION_ITEM('Steel','Steel');
#8891=DESCRIPTIVE_REPRESENTATION_ITEM('Steel','Steel');
#8892=DESCRIPTIVE_REPRESENTATION_ITEM('Steel','Steel');
#8893=DESCRIPTIVE_REPRESENTATION_ITEM('Steel','Steel');
#8894=PROPERTY_DEFINITION('material property','material name',#22185);
#8895=PROPERTY_DEFINITION('material property','density of part',#22185);
#8896=PROPERTY_DEFINITION('material property','material name',#22186);
#8897=PROPERTY_DEFINITION('material property','density of part',#22186);
#8898=PROPERTY_DEFINITION('material property','material name',#22187);
#8899=PROPERTY_DEFINITION('material property','density of part',#22187);
#8900=PROPERTY_DEFINITION('material property','material name',#22189);
#8901=PROPERTY_DEFINITION('material property','density of part',#22189);
#8902=PROPERTY_DEFINITION('material property','material name',#22190);
#8903=PROPERTY_DEFINITION('material property','density of part',#22190);
#8904=PROPERTY_DEFINITION('material property','material name',#22191);
#8905=PROPERTY_DEFINITION('material property','density of part',#22191);
#8906=PROPERTY_DEFINITION('material property','material name',#22192);
#8907=PROPERTY_DEFINITION('material property','density of part',#22192);
#8908=PROPERTY_DEFINITION('material property','material name',#22193);
#8909=PROPERTY_DEFINITION('material property','density of part',#22193);
#8910=PROPERTY_DEFINITION('material property','material name',#22194);
#8911=PROPERTY_DEFINITION('material property','density of part',#22194);
#8912=AXIS2_PLACEMENT_3D('',#11406,#9500,#9501);
#8913=AXIS2_PLACEMENT_3D('',#11407,#9502,#9503);
#8914=AXIS2_PLACEMENT_3D('',#11408,#9504,#9505);
#8915=AXIS2_PLACEMENT_3D('',#11410,#9506,#9507);
#8916=AXIS2_PLACEMENT_3D('',#11413,#9509,#9510);
#8917=AXIS2_PLACEMENT_3D('',#11414,#9511,#9512);
#8918=AXIS2_PLACEMENT_3D('',#11416,#9513,#9514);
#8919=AXIS2_PLACEMENT_3D('',#11419,#9516,#9517);
#8920=AXIS2_PLACEMENT_3D('',#11420,#9518,#9519);
#8921=AXIS2_PLACEMENT_3D('',#11422,#9520,#9521);
#8922=AXIS2_PLACEMENT_3D('',#11425,#9523,#9524);
#8923=AXIS2_PLACEMENT_3D('',#11426,#9525,#9526);
#8924=AXIS2_PLACEMENT_3D('',#11435,#9531,#9532);
#8925=AXIS2_PLACEMENT_3D('',#11441,#9536,#9537);
#8926=AXIS2_PLACEMENT_3D('',#11450,#9542,#9543);
#8927=AXIS2_PLACEMENT_3D('',#11456,#9547,#9548);
#8928=AXIS2_PLACEMENT_3D('',#11465,#9553,#9554);
#8929=AXIS2_PLACEMENT_3D('',#11471,#9558,#9559);
#8930=AXIS2_PLACEMENT_3D('',#11480,#9564,#9565);
#8931=AXIS2_PLACEMENT_3D('',#11486,#9569,#9570);
#8932=AXIS2_PLACEMENT_3D('',#11495,#9575,#9576);
#8933=AXIS2_PLACEMENT_3D('',#11501,#9580,#9581);
#8934=AXIS2_PLACEMENT_3D('',#11510,#9586,#9587);
#8935=AXIS2_PLACEMENT_3D('',#11516,#9591,#9592);
#8936=AXIS2_PLACEMENT_3D('',#11525,#9597,#9598);
#8937=AXIS2_PLACEMENT_3D('',#11531,#9602,#9603);
#8938=AXIS2_PLACEMENT_3D('',#11540,#9608,#9609);
#8939=AXIS2_PLACEMENT_3D('',#11546,#9613,#9614);
#8940=AXIS2_PLACEMENT_3D('',#11555,#9619,#9620);
#8941=AXIS2_PLACEMENT_3D('',#11561,#9624,#9625);
#8942=AXIS2_PLACEMENT_3D('',#11570,#9630,#9631);
#8943=AXIS2_PLACEMENT_3D('',#11576,#9635,#9636);
#8944=AXIS2_PLACEMENT_3D('',#11585,#9641,#9642);
#8945=AXIS2_PLACEMENT_3D('',#11591,#9646,#9647);
#8946=AXIS2_PLACEMENT_3D('',#11600,#9652,#9653);
#8947=AXIS2_PLACEMENT_3D('',#11606,#9657,#9658);
#8948=AXIS2_PLACEMENT_3D('',#11615,#9663,#9664);
#8949=AXIS2_PLACEMENT_3D('',#11621,#9668,#9669);
#8950=AXIS2_PLACEMENT_3D('',#11630,#9674,#9675);
#8951=AXIS2_PLACEMENT_3D('',#11636,#9679,#9680);
#8952=AXIS2_PLACEMENT_3D('',#11645,#9685,#9686);
#8953=AXIS2_PLACEMENT_3D('',#11651,#9690,#9691);
#8954=AXIS2_PLACEMENT_3D('',#11660,#9696,#9697);
#8955=AXIS2_PLACEMENT_3D('',#11666,#9701,#9702);
#8956=AXIS2_PLACEMENT_3D('',#11675,#9707,#9708);
#8957=AXIS2_PLACEMENT_3D('',#11681,#9712,#9713);
#8958=AXIS2_PLACEMENT_3D('',#11690,#9718,#9719);
#8959=AXIS2_PLACEMENT_3D('',#11696,#9723,#9724);
#8960=AXIS2_PLACEMENT_3D('',#11705,#9729,#9730);
#8961=AXIS2_PLACEMENT_3D('',#11711,#9734,#9735);
#8962=AXIS2_PLACEMENT_3D('',#11720,#9740,#9741);
#8963=AXIS2_PLACEMENT_3D('',#11726,#9745,#9746);
#8964=AXIS2_PLACEMENT_3D('',#11735,#9751,#9752);
#8965=AXIS2_PLACEMENT_3D('',#11741,#9756,#9757);
#8966=AXIS2_PLACEMENT_3D('',#11750,#9762,#9763);
#8967=AXIS2_PLACEMENT_3D('',#11756,#9767,#9768);
#8968=AXIS2_PLACEMENT_3D('',#11765,#9773,#9774);
#8969=AXIS2_PLACEMENT_3D('',#11771,#9778,#9779);
#8970=AXIS2_PLACEMENT_3D('',#11780,#9784,#9785);
#8971=AXIS2_PLACEMENT_3D('',#11786,#9789,#9790);
#8972=AXIS2_PLACEMENT_3D('',#11795,#9795,#9796);
#8973=AXIS2_PLACEMENT_3D('',#11801,#9800,#9801);
#8974=AXIS2_PLACEMENT_3D('',#11810,#9806,#9807);
#8975=AXIS2_PLACEMENT_3D('',#11816,#9811,#9812);
#8976=AXIS2_PLACEMENT_3D('',#11825,#9817,#9818);
#8977=AXIS2_PLACEMENT_3D('',#11831,#9822,#9823);
#8978=AXIS2_PLACEMENT_3D('',#11840,#9828,#9829);
#8979=AXIS2_PLACEMENT_3D('',#11846,#9833,#9834);
#8980=AXIS2_PLACEMENT_3D('',#11855,#9839,#9840);
#8981=AXIS2_PLACEMENT_3D('',#11861,#9844,#9845);
#8982=AXIS2_PLACEMENT_3D('',#11870,#9850,#9851);
#8983=AXIS2_PLACEMENT_3D('',#11876,#9855,#9856);
#8984=AXIS2_PLACEMENT_3D('',#11885,#9861,#9862);
#8985=AXIS2_PLACEMENT_3D('',#11891,#9866,#9867);
#8986=AXIS2_PLACEMENT_3D('',#11900,#9872,#9873);
#8987=AXIS2_PLACEMENT_3D('',#11906,#9877,#9878);
#8988=AXIS2_PLACEMENT_3D('',#11915,#9883,#9884);
#8989=AXIS2_PLACEMENT_3D('',#11921,#9888,#9889);
#8990=AXIS2_PLACEMENT_3D('',#11930,#9894,#9895);
#8991=AXIS2_PLACEMENT_3D('',#11936,#9899,#9900);
#8992=AXIS2_PLACEMENT_3D('',#11945,#9905,#9906);
#8993=AXIS2_PLACEMENT_3D('',#11951,#9910,#9911);
#8994=AXIS2_PLACEMENT_3D('',#11960,#9916,#9917);
#8995=AXIS2_PLACEMENT_3D('',#11966,#9921,#9922);
#8996=AXIS2_PLACEMENT_3D('',#11975,#9927,#9928);
#8997=AXIS2_PLACEMENT_3D('',#11981,#9932,#9933);
#8998=AXIS2_PLACEMENT_3D('',#11990,#9938,#9939);
#8999=AXIS2_PLACEMENT_3D('',#11996,#9943,#9944);
#9000=AXIS2_PLACEMENT_3D('',#12006,#9950,#9951);
#9001=AXIS2_PLACEMENT_3D('',#12009,#9954,#9955);
#9002=AXIS2_PLACEMENT_3D('',#12012,#9958,#9959);
#9003=AXIS2_PLACEMENT_3D('',#12015,#9962,#9963);
#9004=AXIS2_PLACEMENT_3D('',#12018,#9966,#9967);
#9005=AXIS2_PLACEMENT_3D('',#12021,#9970,#9971);
#9006=AXIS2_PLACEMENT_3D('',#12024,#9974,#9975);
#9007=AXIS2_PLACEMENT_3D('',#12027,#9978,#9979);
#9008=AXIS2_PLACEMENT_3D('',#12030,#9982,#9983);
#9009=AXIS2_PLACEMENT_3D('',#12033,#9986,#9987);
#9010=AXIS2_PLACEMENT_3D('',#12036,#9990,#9991);
#9011=AXIS2_PLACEMENT_3D('',#12039,#9994,#9995);
#9012=AXIS2_PLACEMENT_3D('',#12042,#9998,#9999);
#9013=AXIS2_PLACEMENT_3D('',#12045,#10002,#10003);
#9014=AXIS2_PLACEMENT_3D('',#12048,#10006,#10007);
#9015=AXIS2_PLACEMENT_3D('',#12051,#10010,#10011);
#9016=AXIS2_PLACEMENT_3D('',#12054,#10014,#10015);
#9017=AXIS2_PLACEMENT_3D('',#12057,#10018,#10019);
#9018=AXIS2_PLACEMENT_3D('',#12060,#10022,#10023);
#9019=AXIS2_PLACEMENT_3D('',#12063,#10026,#10027);
#9020=AXIS2_PLACEMENT_3D('',#12066,#10030,#10031);
#9021=AXIS2_PLACEMENT_3D('',#12069,#10034,#10035);
#9022=AXIS2_PLACEMENT_3D('',#12072,#10038,#10039);
#9023=AXIS2_PLACEMENT_3D('',#12075,#10042,#10043);
#9024=AXIS2_PLACEMENT_3D('',#12078,#10046,#10047);
#9025=AXIS2_PLACEMENT_3D('',#12081,#10050,#10051);
#9026=AXIS2_PLACEMENT_3D('',#12084,#10054,#10055);
#9027=AXIS2_PLACEMENT_3D('',#12087,#10058,#10059);
#9028=AXIS2_PLACEMENT_3D('',#12090,#10062,#10063);
#9029=AXIS2_PLACEMENT_3D('',#12096,#10067,#10068);
#9030=AXIS2_PLACEMENT_3D('',#12099,#10071,#10072);
#9031=AXIS2_PLACEMENT_3D('',#12102,#10075,#10076);
#9032=AXIS2_PLACEMENT_3D('',#12105,#10079,#10080);
#9033=AXIS2_PLACEMENT_3D('',#12108,#10083,#10084);
#9034=AXIS2_PLACEMENT_3D('',#12111,#10087,#10088);
#9035=AXIS2_PLACEMENT_3D('',#12114,#10091,#10092);
#9036=AXIS2_PLACEMENT_3D('',#12117,#10095,#10096);
#9037=AXIS2_PLACEMENT_3D('',#12120,#10099,#10100);
#9038=AXIS2_PLACEMENT_3D('',#12123,#10103,#10104);
#9039=AXIS2_PLACEMENT_3D('',#12131,#10109,#10110);
#9040=AXIS2_PLACEMENT_3D('',#12135,#10113,#10114);
#9041=AXIS2_PLACEMENT_3D('',#12144,#10119,#10120);
#9042=AXIS2_PLACEMENT_3D('',#12148,#10123,#10124);
#9043=AXIS2_PLACEMENT_3D('',#12152,#10127,#10128);
#9044=AXIS2_PLACEMENT_3D('',#12155,#10131,#10132);
#9045=AXIS2_PLACEMENT_3D('',#12157,#10133,#10134);
#9046=AXIS2_PLACEMENT_3D('',#12170,#10141,#10142);
#9047=AXIS2_PLACEMENT_3D('',#12171,#10143,#10144);
#9048=AXIS2_PLACEMENT_3D('',#12173,#10145,#10146);
#9049=AXIS2_PLACEMENT_3D('',#12175,#10148,#10149);
#9050=AXIS2_PLACEMENT_3D('',#12181,#10153,#10154);
#9051=AXIS2_PLACEMENT_3D('',#12185,#10157,#10158);
#9052=AXIS2_PLACEMENT_3D('',#12189,#10161,#10162);
#9053=AXIS2_PLACEMENT_3D('',#12193,#10165,#10166);
#9054=AXIS2_PLACEMENT_3D('',#12197,#10169,#10170);
#9055=AXIS2_PLACEMENT_3D('',#12199,#10172,#10173);
#9056=AXIS2_PLACEMENT_3D('',#12200,#10174,#10175);
#9057=AXIS2_PLACEMENT_3D('',#12201,#10176,#10177);
#9058=AXIS2_PLACEMENT_3D('',#12202,#10178,#10179);
#9059=AXIS2_PLACEMENT_3D('',#12203,#10180,#10181);
#9060=AXIS2_PLACEMENT_3D('',#12205,#10182,#10183);
#9061=AXIS2_PLACEMENT_3D('',#12208,#10185,#10186);
#9062=AXIS2_PLACEMENT_3D('',#12209,#10187,#10188);
#9063=AXIS2_PLACEMENT_3D('',#12211,#10189,#10190);
#9064=AXIS2_PLACEMENT_3D('',#12212,#10191,#10192);
#9065=AXIS2_PLACEMENT_3D('',#12214,#10193,#10194);
#9066=AXIS2_PLACEMENT_3D('',#12215,#10195,#10196);
#9067=AXIS2_PLACEMENT_3D('',#12217,#10197,#10198);
#9068=AXIS2_PLACEMENT_3D('',#12219,#10200,#10201);
#9069=AXIS2_PLACEMENT_3D('',#12221,#10202,#10203);
#9070=AXIS2_PLACEMENT_3D('',#12223,#10204,#10205);
#9071=AXIS2_PLACEMENT_3D('',#12224,#10206,#10207);
#9072=AXIS2_PLACEMENT_3D('',#12227,#10209,#10210);
#9073=AXIS2_PLACEMENT_3D('',#12228,#10211,#10212);
#9074=AXIS2_PLACEMENT_3D('',#12229,#10213,#10214);
#9075=AXIS2_PLACEMENT_3D('',#12231,#10216,#10217);
#9076=AXIS2_PLACEMENT_3D('',#12232,#10218,#10219);
#9077=AXIS2_PLACEMENT_3D('',#12233,#10220,#10221);
#9078=AXIS2_PLACEMENT_3D('',#12242,#10226,#10227);
#9079=AXIS2_PLACEMENT_3D('',#12251,#10232,#10233);
#9080=AXIS2_PLACEMENT_3D('',#12252,#10234,#10235);
#9081=AXIS2_PLACEMENT_3D('',#12253,#10236,#10237);
#9082=AXIS2_PLACEMENT_3D('',#12254,#10238,#10239);
#9083=AXIS2_PLACEMENT_3D('',#12255,#10240,#10241);
#9084=AXIS2_PLACEMENT_3D('',#12256,#10242,#10243);
#9085=AXIS2_PLACEMENT_3D('',#12257,#10244,#10245);
#9086=AXIS2_PLACEMENT_3D('',#12258,#10246,#10247);
#9087=AXIS2_PLACEMENT_3D('',#12259,#10248,#10249);
#9088=AXIS2_PLACEMENT_3D('',#12260,#10250,#10251);
#9089=AXIS2_PLACEMENT_3D('',#12261,#10252,#10253);
#9090=AXIS2_PLACEMENT_3D('',#12288,#10254,#10255);
#9091=AXIS2_PLACEMENT_3D('',#12289,#10256,#10257);
#9092=AXIS2_PLACEMENT_3D('',#12312,#10258,#10259);
#9093=AXIS2_PLACEMENT_3D('',#12313,#10260,#10261);
#9094=AXIS2_PLACEMENT_3D('',#12336,#10262,#10263);
#9095=AXIS2_PLACEMENT_3D('',#12337,#10264,#10265);
#9096=AXIS2_PLACEMENT_3D('',#12364,#10266,#10267);
#9097=AXIS2_PLACEMENT_3D('',#12549,#10268,#10269);
#9098=AXIS2_PLACEMENT_3D('',#12563,#10272,#10273);
#9099=AXIS2_PLACEMENT_3D('',#12565,#10274,#10275);
#9100=AXIS2_PLACEMENT_3D('',#12567,#10276,#10277);
#9101=AXIS2_PLACEMENT_3D('',#12568,#10278,#10279);
#9102=AXIS2_PLACEMENT_3D('',#12570,#10280,#10281);
#9103=AXIS2_PLACEMENT_3D('',#12572,#10283,#10284);
#9104=AXIS2_PLACEMENT_3D('',#12574,#10285,#10286);
#9105=AXIS2_PLACEMENT_3D('',#12577,#10288,#10289);
#9106=AXIS2_PLACEMENT_3D('',#12578,#10290,#10291);
#9107=AXIS2_PLACEMENT_3D('',#12580,#10292,#10293);
#9108=AXIS2_PLACEMENT_3D('',#12583,#10295,#10296);
#9109=AXIS2_PLACEMENT_3D('',#12584,#10297,#10298);
#9110=AXIS2_PLACEMENT_3D('',#12586,#10299,#10300);
#9111=AXIS2_PLACEMENT_3D('',#12588,#10302,#10303);
#9112=AXIS2_PLACEMENT_3D('',#12590,#10304,#10305);
#9113=AXIS2_PLACEMENT_3D('',#12593,#10307,#10308);
#9114=AXIS2_PLACEMENT_3D('',#12594,#10309,#10310);
#9115=AXIS2_PLACEMENT_3D('',#12596,#10311,#10312);
#9116=AXIS2_PLACEMENT_3D('',#12597,#10313,#10314);
#9117=AXIS2_PLACEMENT_3D('',#12599,#10315,#10316);
#9118=AXIS2_PLACEMENT_3D('',#12602,#10318,#10319);
#9119=AXIS2_PLACEMENT_3D('',#12603,#10320,#10321);
#9120=AXIS2_PLACEMENT_3D('',#12605,#10322,#10323);
#9121=AXIS2_PLACEMENT_3D('',#12606,#10324,#10325);
#9122=AXIS2_PLACEMENT_3D('',#12609,#10327,#10328);
#9123=AXIS2_PLACEMENT_3D('',#12610,#10329,#10330);
#9124=AXIS2_PLACEMENT_3D('',#12613,#10332,#10333);
#9125=AXIS2_PLACEMENT_3D('',#12614,#10334,#10335);
#9126=AXIS2_PLACEMENT_3D('',#12623,#10340,#10341);
#9127=AXIS2_PLACEMENT_3D('',#12632,#10346,#10347);
#9128=AXIS2_PLACEMENT_3D('',#12641,#10352,#10353);
#9129=AXIS2_PLACEMENT_3D('',#12650,#10358,#10359);
#9130=AXIS2_PLACEMENT_3D('',#12659,#10364,#10365);
#9131=AXIS2_PLACEMENT_3D('',#12668,#10370,#10371);
#9132=AXIS2_PLACEMENT_3D('',#12677,#10376,#10377);
#9133=AXIS2_PLACEMENT_3D('',#12679,#10378,#10379);
#9134=AXIS2_PLACEMENT_3D('',#12680,#10380,#10381);
#9135=AXIS2_PLACEMENT_3D('',#12682,#10382,#10383);
#9136=AXIS2_PLACEMENT_3D('',#12683,#10384,#10385);
#9137=AXIS2_PLACEMENT_3D('',#12686,#10388,#10389);
#9138=AXIS2_PLACEMENT_3D('',#12689,#10392,#10393);
#9139=AXIS2_PLACEMENT_3D('',#12692,#10396,#10397);
#9140=AXIS2_PLACEMENT_3D('',#12698,#10401,#10402);
#9141=AXIS2_PLACEMENT_3D('',#12704,#10406,#10407);
#9142=AXIS2_PLACEMENT_3D('',#12749,#10409,#10410);
#9143=AXIS2_PLACEMENT_3D('',#12795,#10413,#10414);
#9144=AXIS2_PLACEMENT_3D('',#12873,#10418,#10419);
#9145=AXIS2_PLACEMENT_3D('',#12921,#10423,#10424);
#9146=AXIS2_PLACEMENT_3D('',#12937,#10428,#10429);
#9147=AXIS2_PLACEMENT_3D('',#13258,#10441,#10442);
#9148=AXIS2_PLACEMENT_3D('',#13260,#10444,#10445);
#9149=AXIS2_PLACEMENT_3D('',#13262,#10446,#10447);
#9150=AXIS2_PLACEMENT_3D('',#13264,#10449,#10450);
#9151=AXIS2_PLACEMENT_3D('',#13428,#10452,#10453);
#9152=AXIS2_PLACEMENT_3D('',#13429,#10454,#10455);
#9153=AXIS2_PLACEMENT_3D('',#13477,#10457,#10458);
#9154=AXIS2_PLACEMENT_3D('',#13595,#10460,#10461);
#9155=AXIS2_PLACEMENT_3D('',#13640,#10462,#10463);
#9156=AXIS2_PLACEMENT_3D('',#13732,#10465,#10466);
#9157=AXIS2_PLACEMENT_3D('',#13749,#10467,#10468);
#9158=AXIS2_PLACEMENT_3D('',#13869,#10470,#10471);
#9159=AXIS2_PLACEMENT_3D('',#13874,#10472,#10473);
#9160=AXIS2_PLACEMENT_3D('',#13926,#10475,#10476);
#9161=AXIS2_PLACEMENT_3D('',#13927,#10477,#10478);
#9162=AXIS2_PLACEMENT_3D('',#13928,#10479,#10480);
#9163=AXIS2_PLACEMENT_3D('',#13929,#10481,#10482);
#9164=AXIS2_PLACEMENT_3D('',#13930,#10483,#10484);
#9165=AXIS2_PLACEMENT_3D('',#13931,#10485,#10486);
#9166=AXIS2_PLACEMENT_3D('',#13933,#10487,#10488);
#9167=AXIS2_PLACEMENT_3D('',#13934,#10489,#10490);
#9168=AXIS2_PLACEMENT_3D('',#13935,#10491,#10492);
#9169=AXIS2_PLACEMENT_3D('',#13936,#10493,#10494);
#9170=AXIS2_PLACEMENT_3D('',#13937,#10495,#10496);
#9171=AXIS2_PLACEMENT_3D('',#13938,#10497,#10498);
#9172=AXIS2_PLACEMENT_3D('',#13959,#10499,#10500);
#9173=AXIS2_PLACEMENT_3D('',#13961,#10501,#10502);
#9174=AXIS2_PLACEMENT_3D('',#13962,#10503,#10504);
#9175=AXIS2_PLACEMENT_3D('',#13963,#10505,#10506);
#9176=AXIS2_PLACEMENT_3D('',#14053,#10508,#10509);
#9177=AXIS2_PLACEMENT_3D('',#14054,#10510,#10511);
#9178=AXIS2_PLACEMENT_3D('',#14057,#10512,#10513);
#9179=AXIS2_PLACEMENT_3D('',#14059,#10514,#10515);
#9180=AXIS2_PLACEMENT_3D('',#14060,#10516,#10517);
#9181=AXIS2_PLACEMENT_3D('',#14061,#10518,#10519);
#9182=AXIS2_PLACEMENT_3D('',#14064,#10520,#10521);
#9183=AXIS2_PLACEMENT_3D('',#14066,#10522,#10523);
#9184=AXIS2_PLACEMENT_3D('',#14067,#10524,#10525);
#9185=AXIS2_PLACEMENT_3D('',#14068,#10526,#10527);
#9186=AXIS2_PLACEMENT_3D('',#14071,#10528,#10529);
#9187=AXIS2_PLACEMENT_3D('',#14073,#10530,#10531);
#9188=AXIS2_PLACEMENT_3D('',#14074,#10532,#10533);
#9189=AXIS2_PLACEMENT_3D('',#14075,#10534,#10535);
#9190=AXIS2_PLACEMENT_3D('',#14106,#10538,#10539);
#9191=AXIS2_PLACEMENT_3D('',#14109,#10540,#10541);
#9192=AXIS2_PLACEMENT_3D('',#14111,#10542,#10543);
#9193=AXIS2_PLACEMENT_3D('',#14112,#10544,#10545);
#9194=AXIS2_PLACEMENT_3D('',#14113,#10546,#10547);
#9195=AXIS2_PLACEMENT_3D('',#14286,#10550,#10551);
#9196=AXIS2_PLACEMENT_3D('',#14287,#10552,#10553);
#9197=AXIS2_PLACEMENT_3D('',#14304,#10554,#10555);
#9198=AXIS2_PLACEMENT_3D('',#14305,#10556,#10557);
#9199=AXIS2_PLACEMENT_3D('',#14306,#10558,#10559);
#9200=AXIS2_PLACEMENT_3D('',#14333,#10560,#10561);
#9201=AXIS2_PLACEMENT_3D('',#14334,#10562,#10563);
#9202=AXIS2_PLACEMENT_3D('',#14357,#10564,#10565);
#9203=AXIS2_PLACEMENT_3D('',#14358,#10566,#10567);
#9204=AXIS2_PLACEMENT_3D('',#14381,#10568,#10569);
#9205=AXIS2_PLACEMENT_3D('',#14382,#10570,#10571);
#9206=AXIS2_PLACEMENT_3D('',#14409,#10572,#10573);
#9207=AXIS2_PLACEMENT_3D('',#14594,#10574,#10575);
#9208=AXIS2_PLACEMENT_3D('',#14608,#10578,#10579);
#9209=AXIS2_PLACEMENT_3D('',#14610,#10580,#10581);
#9210=AXIS2_PLACEMENT_3D('',#14612,#10582,#10583);
#9211=AXIS2_PLACEMENT_3D('',#14613,#10584,#10585);
#9212=AXIS2_PLACEMENT_3D('',#14622,#10590,#10591);
#9213=AXIS2_PLACEMENT_3D('',#14628,#10595,#10596);
#9214=AXIS2_PLACEMENT_3D('',#14634,#10600,#10601);
#9215=AXIS2_PLACEMENT_3D('',#14640,#10605,#10606);
#9216=AXIS2_PLACEMENT_3D('',#14646,#10610,#10611);
#9217=AXIS2_PLACEMENT_3D('',#14649,#10614,#10615);
#9218=AXIS2_PLACEMENT_3D('',#14651,#10616,#10617);
#9219=AXIS2_PLACEMENT_3D('',#14652,#10618,#10619);
#9220=AXIS2_PLACEMENT_3D('',#14661,#10624,#10625);
#9221=AXIS2_PLACEMENT_3D('',#14667,#10629,#10630);
#9222=AXIS2_PLACEMENT_3D('',#14673,#10634,#10635);
#9223=AXIS2_PLACEMENT_3D('',#14679,#10639,#10640);
#9224=AXIS2_PLACEMENT_3D('',#14685,#10644,#10645);
#9225=AXIS2_PLACEMENT_3D('',#14688,#10648,#10649);
#9226=AXIS2_PLACEMENT_3D('',#14690,#10650,#10651);
#9227=AXIS2_PLACEMENT_3D('',#14691,#10652,#10653);
#9228=AXIS2_PLACEMENT_3D('',#14693,#10654,#10655);
#9229=AXIS2_PLACEMENT_3D('',#14695,#10657,#10658);
#9230=AXIS2_PLACEMENT_3D('',#14697,#10659,#10660);
#9231=AXIS2_PLACEMENT_3D('',#14700,#10662,#10663);
#9232=AXIS2_PLACEMENT_3D('',#14701,#10664,#10665);
#9233=AXIS2_PLACEMENT_3D('',#14703,#10666,#10667);
#9234=AXIS2_PLACEMENT_3D('',#14706,#10669,#10670);
#9235=AXIS2_PLACEMENT_3D('',#14707,#10671,#10672);
#9236=AXIS2_PLACEMENT_3D('',#14709,#10673,#10674);
#9237=AXIS2_PLACEMENT_3D('',#14711,#10676,#10677);
#9238=AXIS2_PLACEMENT_3D('',#14714,#10679,#10680);
#9239=AXIS2_PLACEMENT_3D('',#14715,#10681,#10682);
#9240=AXIS2_PLACEMENT_3D('',#14718,#10684,#10685);
#9241=AXIS2_PLACEMENT_3D('',#14719,#10686,#10687);
#9242=AXIS2_PLACEMENT_3D('',#14728,#10692,#10693);
#9243=AXIS2_PLACEMENT_3D('',#14737,#10698,#10699);
#9244=AXIS2_PLACEMENT_3D('',#14746,#10704,#10705);
#9245=AXIS2_PLACEMENT_3D('',#14755,#10710,#10711);
#9246=AXIS2_PLACEMENT_3D('',#14764,#10716,#10717);
#9247=AXIS2_PLACEMENT_3D('',#14773,#10722,#10723);
#9248=AXIS2_PLACEMENT_3D('',#14782,#10728,#10729);
#9249=AXIS2_PLACEMENT_3D('',#14784,#10730,#10731);
#9250=AXIS2_PLACEMENT_3D('',#14785,#10732,#10733);
#9251=AXIS2_PLACEMENT_3D('',#14787,#10734,#10735);
#9252=AXIS2_PLACEMENT_3D('',#14788,#10736,#10737);
#9253=AXIS2_PLACEMENT_3D('',#14791,#10740,#10741);
#9254=AXIS2_PLACEMENT_3D('',#14794,#10744,#10745);
#9255=AXIS2_PLACEMENT_3D('',#14797,#10748,#10749);
#9256=AXIS2_PLACEMENT_3D('',#14803,#10753,#10754);
#9257=AXIS2_PLACEMENT_3D('',#14809,#10758,#10759);
#9258=AXIS2_PLACEMENT_3D('',#14854,#10761,#10762);
#9259=AXIS2_PLACEMENT_3D('',#14900,#10765,#10766);
#9260=AXIS2_PLACEMENT_3D('',#14978,#10770,#10771);
#9261=AXIS2_PLACEMENT_3D('',#15026,#10775,#10776);
#9262=AXIS2_PLACEMENT_3D('',#15042,#10780,#10781);
#9263=AXIS2_PLACEMENT_3D('',#15363,#10793,#10794);
#9264=AXIS2_PLACEMENT_3D('',#15365,#10796,#10797);
#9265=AXIS2_PLACEMENT_3D('',#15367,#10798,#10799);
#9266=AXIS2_PLACEMENT_3D('',#15369,#10801,#10802);
#9267=AXIS2_PLACEMENT_3D('',#15533,#10804,#10805);
#9268=AXIS2_PLACEMENT_3D('',#15534,#10806,#10807);
#9269=AXIS2_PLACEMENT_3D('',#15582,#10809,#10810);
#9270=AXIS2_PLACEMENT_3D('',#15700,#10812,#10813);
#9271=AXIS2_PLACEMENT_3D('',#15745,#10814,#10815);
#9272=AXIS2_PLACEMENT_3D('',#15837,#10817,#10818);
#9273=AXIS2_PLACEMENT_3D('',#15854,#10819,#10820);
#9274=AXIS2_PLACEMENT_3D('',#15974,#10822,#10823);
#9275=AXIS2_PLACEMENT_3D('',#15979,#10824,#10825);
#9276=AXIS2_PLACEMENT_3D('',#16031,#10827,#10828);
#9277=AXIS2_PLACEMENT_3D('',#16032,#10829,#10830);
#9278=AXIS2_PLACEMENT_3D('',#16033,#10831,#10832);
#9279=AXIS2_PLACEMENT_3D('',#16034,#10833,#10834);
#9280=AXIS2_PLACEMENT_3D('',#16035,#10835,#10836);
#9281=AXIS2_PLACEMENT_3D('',#16036,#10837,#10838);
#9282=AXIS2_PLACEMENT_3D('',#16038,#10839,#10840);
#9283=AXIS2_PLACEMENT_3D('',#16039,#10841,#10842);
#9284=AXIS2_PLACEMENT_3D('',#16040,#10843,#10844);
#9285=AXIS2_PLACEMENT_3D('',#16041,#10845,#10846);
#9286=AXIS2_PLACEMENT_3D('',#16042,#10847,#10848);
#9287=AXIS2_PLACEMENT_3D('',#16043,#10849,#10850);
#9288=AXIS2_PLACEMENT_3D('',#16064,#10851,#10852);
#9289=AXIS2_PLACEMENT_3D('',#16066,#10853,#10854);
#9290=AXIS2_PLACEMENT_3D('',#16067,#10855,#10856);
#9291=AXIS2_PLACEMENT_3D('',#16068,#10857,#10858);
#9292=AXIS2_PLACEMENT_3D('',#16158,#10860,#10861);
#9293=AXIS2_PLACEMENT_3D('',#16159,#10862,#10863);
#9294=AXIS2_PLACEMENT_3D('',#16162,#10864,#10865);
#9295=AXIS2_PLACEMENT_3D('',#16164,#10866,#10867);
#9296=AXIS2_PLACEMENT_3D('',#16165,#10868,#10869);
#9297=AXIS2_PLACEMENT_3D('',#16166,#10870,#10871);
#9298=AXIS2_PLACEMENT_3D('',#16169,#10872,#10873);
#9299=AXIS2_PLACEMENT_3D('',#16171,#10874,#10875);
#9300=AXIS2_PLACEMENT_3D('',#16172,#10876,#10877);
#9301=AXIS2_PLACEMENT_3D('',#16173,#10878,#10879);
#9302=AXIS2_PLACEMENT_3D('',#16176,#10880,#10881);
#9303=AXIS2_PLACEMENT_3D('',#16178,#10882,#10883);
#9304=AXIS2_PLACEMENT_3D('',#16179,#10884,#10885);
#9305=AXIS2_PLACEMENT_3D('',#16180,#10886,#10887);
#9306=AXIS2_PLACEMENT_3D('',#16211,#10890,#10891);
#9307=AXIS2_PLACEMENT_3D('',#16214,#10892,#10893);
#9308=AXIS2_PLACEMENT_3D('',#16216,#10894,#10895);
#9309=AXIS2_PLACEMENT_3D('',#16217,#10896,#10897);
#9310=AXIS2_PLACEMENT_3D('',#16218,#10898,#10899);
#9311=AXIS2_PLACEMENT_3D('',#16391,#10902,#10903);
#9312=AXIS2_PLACEMENT_3D('',#16392,#10904,#10905);
#9313=AXIS2_PLACEMENT_3D('',#16409,#10906,#10907);
#9314=AXIS2_PLACEMENT_3D('',#16410,#10908,#10909);
#9315=AXIS2_PLACEMENT_3D('',#16411,#10910,#10911);
#9316=AXIS2_PLACEMENT_3D('',#16427,#10913,#10914);
#9317=AXIS2_PLACEMENT_3D('',#16435,#10915,#10916);
#9318=AXIS2_PLACEMENT_3D('',#16483,#10918,#10919);
#9319=AXIS2_PLACEMENT_3D('',#16531,#10921,#10922);
#9320=AXIS2_PLACEMENT_3D('',#16582,#10924,#10925);
#9321=AXIS2_PLACEMENT_3D('',#16630,#10927,#10928);
#9322=AXIS2_PLACEMENT_3D('',#16678,#10930,#10931);
#9323=AXIS2_PLACEMENT_3D('',#16726,#10933,#10934);
#9324=AXIS2_PLACEMENT_3D('',#16780,#10936,#10937);
#9325=AXIS2_PLACEMENT_3D('',#16828,#10939,#10940);
#9326=AXIS2_PLACEMENT_3D('',#16876,#10942,#10943);
#9327=AXIS2_PLACEMENT_3D('',#16930,#10945,#10946);
#9328=AXIS2_PLACEMENT_3D('',#16978,#10948,#10949);
#9329=AXIS2_PLACEMENT_3D('',#17026,#10951,#10952);
#9330=AXIS2_PLACEMENT_3D('',#17074,#10954,#10955);
#9331=AXIS2_PLACEMENT_3D('',#17128,#10957,#10958);
#9332=AXIS2_PLACEMENT_3D('',#17176,#10960,#10961);
#9333=AXIS2_PLACEMENT_3D('',#17224,#10963,#10964);
#9334=AXIS2_PLACEMENT_3D('',#17278,#10966,#10967);
#9335=AXIS2_PLACEMENT_3D('',#17326,#10969,#10970);
#9336=AXIS2_PLACEMENT_3D('',#17374,#10972,#10973);
#9337=AXIS2_PLACEMENT_3D('',#17428,#10975,#10976);
#9338=AXIS2_PLACEMENT_3D('',#17476,#10978,#10979);
#9339=AXIS2_PLACEMENT_3D('',#17524,#10981,#10982);
#9340=AXIS2_PLACEMENT_3D('',#17572,#10984,#10985);
#9341=AXIS2_PLACEMENT_3D('',#17626,#10987,#10988);
#9342=AXIS2_PLACEMENT_3D('',#17674,#10990,#10991);
#9343=AXIS2_PLACEMENT_3D('',#17722,#10993,#10994);
#9344=AXIS2_PLACEMENT_3D('',#17776,#10996,#10997);
#9345=AXIS2_PLACEMENT_3D('',#17824,#10999,#11000);
#9346=AXIS2_PLACEMENT_3D('',#17872,#11002,#11003);
#9347=AXIS2_PLACEMENT_3D('',#17888,#11005,#11006);
#9348=AXIS2_PLACEMENT_3D('',#17898,#11007,#11008);
#9349=AXIS2_PLACEMENT_3D('',#17922,#11010,#11011);
#9350=AXIS2_PLACEMENT_3D('',#17946,#11013,#11014);
#9351=AXIS2_PLACEMENT_3D('',#17971,#11016,#11017);
#9352=AXIS2_PLACEMENT_3D('',#17996,#11019,#11020);
#9353=AXIS2_PLACEMENT_3D('',#18020,#11022,#11023);
#9354=AXIS2_PLACEMENT_3D('',#18045,#11025,#11026);
#9355=AXIS2_PLACEMENT_3D('',#18070,#11028,#11029);
#9356=AXIS2_PLACEMENT_3D('',#18094,#11031,#11032);
#9357=AXIS2_PLACEMENT_3D('',#18118,#11034,#11035);
#9358=AXIS2_PLACEMENT_3D('',#18143,#11037,#11038);
#9359=AXIS2_PLACEMENT_3D('',#18168,#11040,#11041);
#9360=AXIS2_PLACEMENT_3D('',#18192,#11043,#11044);
#9361=AXIS2_PLACEMENT_3D('',#18217,#11046,#11047);
#9362=AXIS2_PLACEMENT_3D('',#18242,#11049,#11050);
#9363=AXIS2_PLACEMENT_3D('',#18266,#11052,#11053);
#9364=AXIS2_PLACEMENT_3D('',#18291,#11055,#11056);
#9365=AXIS2_PLACEMENT_3D('',#18316,#11058,#11059);
#9366=AXIS2_PLACEMENT_3D('',#18340,#11061,#11062);
#9367=AXIS2_PLACEMENT_3D('',#18364,#11064,#11065);
#9368=AXIS2_PLACEMENT_3D('',#18389,#11067,#11068);
#9369=AXIS2_PLACEMENT_3D('',#18414,#11070,#11071);
#9370=AXIS2_PLACEMENT_3D('',#18438,#11073,#11074);
#9371=AXIS2_PLACEMENT_3D('',#18463,#11076,#11077);
#9372=AXIS2_PLACEMENT_3D('',#18488,#11079,#11080);
#9373=AXIS2_PLACEMENT_3D('',#18512,#11082,#11083);
#9374=AXIS2_PLACEMENT_3D('',#18537,#11085,#11086);
#9375=AXIS2_PLACEMENT_3D('',#18561,#11088,#11089);
#9376=AXIS2_PLACEMENT_3D('',#18586,#11091,#11092);
#9377=AXIS2_PLACEMENT_3D('',#18610,#11094,#11095);
#9378=AXIS2_PLACEMENT_3D('',#18772,#11096,#11097);
#9379=AXIS2_PLACEMENT_3D('',#18791,#11099,#11100);
#9380=AXIS2_PLACEMENT_3D('',#19653,#11101,#11102);
#9381=AXIS2_PLACEMENT_3D('',#19664,#11103,#11104);
#9382=AXIS2_PLACEMENT_3D('',#20531,#11105,#11106);
#9383=AXIS2_PLACEMENT_3D('',#20532,#11107,#11108);
#9384=AXIS2_PLACEMENT_3D('',#20541,#11113,#11114);
#9385=AXIS2_PLACEMENT_3D('',#20547,#11118,#11119);
#9386=AXIS2_PLACEMENT_3D('',#20553,#11123,#11124);
#9387=AXIS2_PLACEMENT_3D('',#20559,#11128,#11129);
#9388=AXIS2_PLACEMENT_3D('',#20565,#11133,#11134);
#9389=AXIS2_PLACEMENT_3D('',#20568,#11137,#11138);
#9390=AXIS2_PLACEMENT_3D('',#20569,#11139,#11140);
#9391=AXIS2_PLACEMENT_3D('',#20571,#11141,#11142);
#9392=AXIS2_PLACEMENT_3D('',#20572,#11143,#11144);
#9393=AXIS2_PLACEMENT_3D('',#20575,#11146,#11147);
#9394=AXIS2_PLACEMENT_3D('',#20576,#11148,#11149);
#9395=AXIS2_PLACEMENT_3D('',#20577,#11150,#11151);
#9396=AXIS2_PLACEMENT_3D('',#20578,#11152,#11153);
#9397=AXIS2_PLACEMENT_3D('',#20579,#11154,#11155);
#9398=AXIS2_PLACEMENT_3D('',#20584,#11157,#11158);
#9399=AXIS2_PLACEMENT_3D('',#20592,#11159,#11160);
#9400=AXIS2_PLACEMENT_3D('',#20616,#11162,#11163);
#9401=AXIS2_PLACEMENT_3D('',#20639,#11164,#11165);
#9402=AXIS2_PLACEMENT_3D('',#20693,#11167,#11168);
#9403=AXIS2_PLACEMENT_3D('',#20741,#11170,#11171);
#9404=AXIS2_PLACEMENT_3D('',#20760,#11173,#11174);
#9405=AXIS2_PLACEMENT_3D('',#20780,#11175,#11176);
#9406=AXIS2_PLACEMENT_3D('',#20793,#11178,#11179);
#9407=AXIS2_PLACEMENT_3D('',#20801,#11180,#11181);
#9408=AXIS2_PLACEMENT_3D('',#20826,#11183,#11184);
#9409=AXIS2_PLACEMENT_3D('',#20851,#11186,#11187);
#9410=AXIS2_PLACEMENT_3D('',#20876,#11189,#11190);
#9411=AXIS2_PLACEMENT_3D('',#20887,#11192,#11193);
#9412=AXIS2_PLACEMENT_3D('',#20893,#11194,#11195);
#9413=AXIS2_PLACEMENT_3D('',#21449,#11196,#11197);
#9414=AXIS2_PLACEMENT_3D('',#21462,#11204,#11205);
#9415=AXIS2_PLACEMENT_3D('',#21463,#11206,#11207);
#9416=AXIS2_PLACEMENT_3D('',#21469,#11211,#11212);
#9417=AXIS2_PLACEMENT_3D('',#21473,#11215,#11216);
#9418=AXIS2_PLACEMENT_3D('',#21477,#11219,#11220);
#9419=AXIS2_PLACEMENT_3D('',#21481,#11223,#11224);
#9420=AXIS2_PLACEMENT_3D('',#21485,#11227,#11228);
#9421=AXIS2_PLACEMENT_3D('',#21487,#11230,#11231);
#9422=AXIS2_PLACEMENT_3D('',#21488,#11232,#11233);
#9423=AXIS2_PLACEMENT_3D('',#21489,#11234,#11235);
#9424=AXIS2_PLACEMENT_3D('',#21491,#11236,#11237);
#9425=AXIS2_PLACEMENT_3D('',#21494,#11239,#11240);
#9426=AXIS2_PLACEMENT_3D('',#21495,#11241,#11242);
#9427=AXIS2_PLACEMENT_3D('',#21497,#11243,#11244);
#9428=AXIS2_PLACEMENT_3D('',#21500,#11246,#11247);
#9429=AXIS2_PLACEMENT_3D('',#21501,#11248,#11249);
#9430=AXIS2_PLACEMENT_3D('',#21503,#11250,#11251);
#9431=AXIS2_PLACEMENT_3D('',#21505,#11252,#11253);
#9432=AXIS2_PLACEMENT_3D('',#21506,#11254,#11255);
#9433=AXIS2_PLACEMENT_3D('',#21508,#11256,#11257);
#9434=AXIS2_PLACEMENT_3D('',#21510,#11259,#11260);
#9435=AXIS2_PLACEMENT_3D('',#21511,#11261,#11262);
#9436=AXIS2_PLACEMENT_3D('',#21513,#11263,#11264);
#9437=AXIS2_PLACEMENT_3D('',#21515,#11265,#11266);
#9438=AXIS2_PLACEMENT_3D('',#21516,#11267,#11268);
#9439=AXIS2_PLACEMENT_3D('',#21518,#11269,#11270);
#9440=AXIS2_PLACEMENT_3D('',#21520,#11272,#11273);
#9441=AXIS2_PLACEMENT_3D('',#21521,#11274,#11275);
#9442=AXIS2_PLACEMENT_3D('',#21523,#11276,#11277);
#9443=AXIS2_PLACEMENT_3D('',#21525,#11278,#11279);
#9444=AXIS2_PLACEMENT_3D('',#21526,#11280,#11281);
#9445=AXIS2_PLACEMENT_3D('',#21528,#11282,#11283);
#9446=AXIS2_PLACEMENT_3D('',#21530,#11285,#11286);
#9447=AXIS2_PLACEMENT_3D('',#21531,#11287,#11288);
#9448=AXIS2_PLACEMENT_3D('',#21533,#11289,#11290);
#9449=AXIS2_PLACEMENT_3D('',#21535,#11291,#11292);
#9450=AXIS2_PLACEMENT_3D('',#21536,#11293,#11294);
#9451=AXIS2_PLACEMENT_3D('',#21538,#11295,#11296);
#9452=AXIS2_PLACEMENT_3D('',#21540,#11298,#11299);
#9453=AXIS2_PLACEMENT_3D('',#21541,#11300,#11301);
#9454=AXIS2_PLACEMENT_3D('',#21544,#11303,#11304);
#9455=AXIS2_PLACEMENT_3D('',#21545,#11305,#11306);
#9456=AXIS2_PLACEMENT_3D('',#21548,#11308,#11309);
#9457=AXIS2_PLACEMENT_3D('',#21549,#11310,#11311);
#9458=AXIS2_PLACEMENT_3D('',#21552,#11313,#11314);
#9459=AXIS2_PLACEMENT_3D('',#21553,#11315,#11316);
#9460=AXIS2_PLACEMENT_3D('',#21556,#11318,#11319);
#9461=AXIS2_PLACEMENT_3D('',#21584,#11320,#11321);
#9462=AXIS2_PLACEMENT_3D('',#21592,#11322,#11323);
#9463=AXIS2_PLACEMENT_3D('',#21598,#11324,#11325);
#9464=AXIS2_PLACEMENT_3D('',#21601,#11326,#11327);
#9465=AXIS2_PLACEMENT_3D('',#21631,#11330,#11331);
#9466=AXIS2_PLACEMENT_3D('',#21669,#11332,#11333);
#9467=AXIS2_PLACEMENT_3D('',#21707,#11334,#11335);
#9468=AXIS2_PLACEMENT_3D('',#21718,#11336,#11337);
#9469=AXIS2_PLACEMENT_3D('',#21721,#11338,#11339);
#9470=AXIS2_PLACEMENT_3D('',#21751,#11342,#11343);
#9471=AXIS2_PLACEMENT_3D('',#21797,#11344,#11345);
#9472=AXIS2_PLACEMENT_3D('',#21940,#11347,#11348);
#9473=AXIS2_PLACEMENT_3D('',#21941,#11349,#11350);
#9474=AXIS2_PLACEMENT_3D('',#22054,#11352,#11353);
#9475=AXIS2_PLACEMENT_3D('',#22075,#11354,#11355);
#9476=AXIS2_PLACEMENT_3D('',#22076,#11356,#11357);
#9477=AXIS2_PLACEMENT_3D('',#22077,#11358,#11359);
#9478=AXIS2_PLACEMENT_3D('',#22078,#11360,#11361);
#9479=AXIS2_PLACEMENT_3D('',#22079,#11362,#11363);
#9480=AXIS2_PLACEMENT_3D('',#22080,#11364,#11365);
#9481=AXIS2_PLACEMENT_3D('',#22081,#11366,#11367);
#9482=AXIS2_PLACEMENT_3D('',#22082,#11368,#11369);
#9483=AXIS2_PLACEMENT_3D('',#22083,#11370,#11371);
#9484=AXIS2_PLACEMENT_3D('',#22084,#11372,#11373);
#9485=AXIS2_PLACEMENT_3D('',#22086,#11374,#11375);
#9486=AXIS2_PLACEMENT_3D('',#22089,#11377,#11378);
#9487=AXIS2_PLACEMENT_3D('',#22090,#11379,#11380);
#9488=AXIS2_PLACEMENT_3D('',#22092,#11381,#11382);
#9489=AXIS2_PLACEMENT_3D('',#22095,#11384,#11385);
#9490=AXIS2_PLACEMENT_3D('',#22096,#11386,#11387);
#9491=AXIS2_PLACEMENT_3D('',#22097,#11388,#11389);
#9492=AXIS2_PLACEMENT_3D('',#22098,#11390,#11391);
#9493=AXIS2_PLACEMENT_3D('',#22099,#11392,#11393);
#9494=AXIS2_PLACEMENT_3D('',#22100,#11394,#11395);
#9495=AXIS2_PLACEMENT_3D('',#22101,#11396,#11397);
#9496=AXIS2_PLACEMENT_3D('',#22102,#11398,#11399);
#9497=AXIS2_PLACEMENT_3D('',#22103,#11400,#11401);
#9498=AXIS2_PLACEMENT_3D('',#22104,#11402,#11403);
#9499=AXIS2_PLACEMENT_3D('',#22105,#11404,#11405);
#9500=DIRECTION('axis',(0.,0.,1.));
#9501=DIRECTION('refdir',(1.,0.,0.));
#9502=DIRECTION('axis',(0.,0.,1.));
#9503=DIRECTION('refdir',(1.,0.,0.));
#9504=DIRECTION('center_axis',(0.,0.,-1.));
#9505=DIRECTION('ref_axis',(1.,0.,0.));
#9506=DIRECTION('center_axis',(0.,0.,-1.));
#9507=DIRECTION('ref_axis',(1.,0.,0.));
#9508=DIRECTION('',(0.,0.,-1.));
#9509=DIRECTION('center_axis',(0.,0.,1.));
#9510=DIRECTION('ref_axis',(1.,0.,0.));
#9511=DIRECTION('center_axis',(0.,0.,-1.));
#9512=DIRECTION('ref_axis',(1.,0.,0.));
#9513=DIRECTION('center_axis',(0.,0.,-1.));
#9514=DIRECTION('ref_axis',(1.,0.,0.));
#9515=DIRECTION('',(0.,0.,-1.));
#9516=DIRECTION('center_axis',(0.,0.,1.));
#9517=DIRECTION('ref_axis',(1.,0.,0.));
#9518=DIRECTION('center_axis',(0.,0.,-1.));
#9519=DIRECTION('ref_axis',(1.,0.,0.));
#9520=DIRECTION('center_axis',(0.,0.,-1.));
#9521=DIRECTION('ref_axis',(1.,0.,0.));
#9522=DIRECTION('',(0.,0.,-1.));
#9523=DIRECTION('center_axis',(0.,0.,1.));
#9524=DIRECTION('ref_axis',(1.,0.,0.));
#9525=DIRECTION('center_axis',(0.810679228399881,0.585490553844358,0.));
#9526=DIRECTION('ref_axis',(0.585490553844358,-0.810679228399881,0.));
#9527=DIRECTION('',(0.,0.,-1.));
#9528=DIRECTION('',(0.585490553844358,-0.810679228399881,0.));
#9529=DIRECTION('',(0.,0.,-1.));
#9530=DIRECTION('',(-0.585490553844358,0.810679228399881,0.));
#9531=DIRECTION('center_axis',(-0.810679228399881,0.585490553844358,0.));
#9532=DIRECTION('ref_axis',(0.585490553844358,0.810679228399881,0.));
#9533=DIRECTION('',(0.,0.,1.));
#9534=DIRECTION('',(-0.585490553844358,-0.810679228399881,0.));
#9535=DIRECTION('',(0.585490553844358,0.810679228399881,0.));
#9536=DIRECTION('center_axis',(0.810679228399881,0.585490553844358,0.));
#9537=DIRECTION('ref_axis',(0.585490553844358,-0.810679228399881,0.));
#9538=DIRECTION('',(0.,0.,-1.));
#9539=DIRECTION('',(0.585490553844358,-0.810679228399881,0.));
#9540=DIRECTION('',(0.,0.,-1.));
#9541=DIRECTION('',(-0.585490553844358,0.810679228399881,0.));
#9542=DIRECTION('center_axis',(-0.810679228399881,0.585490553844358,0.));
#9543=DIRECTION('ref_axis',(0.585490553844358,0.810679228399881,0.));
#9544=DIRECTION('',(0.,0.,1.));
#9545=DIRECTION('',(-0.585490553844358,-0.810679228399881,0.));
#9546=DIRECTION('',(0.585490553844358,0.810679228399881,0.));
#9547=DIRECTION('center_axis',(0.810679228399883,0.585490553844356,0.));
#9548=DIRECTION('ref_axis',(0.585490553844356,-0.810679228399883,0.));
#9549=DIRECTION('',(0.,0.,-1.));
#9550=DIRECTION('',(0.585490553844356,-0.810679228399883,0.));
#9551=DIRECTION('',(0.,0.,-1.));
#9552=DIRECTION('',(-0.585490553844356,0.810679228399883,0.));
#9553=DIRECTION('center_axis',(-0.810679228399881,0.585490553844358,0.));
#9554=DIRECTION('ref_axis',(0.585490553844358,0.810679228399881,0.));
#9555=DIRECTION('',(0.,0.,1.));
#9556=DIRECTION('',(-0.585490553844358,-0.810679228399881,0.));
#9557=DIRECTION('',(0.585490553844358,0.810679228399881,0.));
#9558=DIRECTION('center_axis',(0.810679228399879,0.585490553844361,0.));
#9559=DIRECTION('ref_axis',(0.585490553844361,-0.810679228399879,0.));
#9560=DIRECTION('',(0.,0.,-1.));
#9561=DIRECTION('',(0.585490553844361,-0.810679228399879,0.));
#9562=DIRECTION('',(0.,0.,-1.));
#9563=DIRECTION('',(-0.585490553844361,0.810679228399879,0.));
#9564=DIRECTION('center_axis',(-0.810679228399883,0.585490553844356,0.));
#9565=DIRECTION('ref_axis',(0.585490553844356,0.810679228399883,0.));
#9566=DIRECTION('',(0.,0.,1.));
#9567=DIRECTION('',(-0.585490553844356,-0.810679228399883,0.));
#9568=DIRECTION('',(0.585490553844356,0.810679228399883,0.));
#9569=DIRECTION('center_axis',(0.810679228399883,0.585490553844356,0.));
#9570=DIRECTION('ref_axis',(0.585490553844356,-0.810679228399883,0.));
#9571=DIRECTION('',(0.,0.,-1.));
#9572=DIRECTION('',(0.585490553844356,-0.810679228399883,0.));
#9573=DIRECTION('',(0.,0.,-1.));
#9574=DIRECTION('',(-0.585490553844356,0.810679228399883,0.));
#9575=DIRECTION('center_axis',(-0.810679228399879,0.585490553844361,0.));
#9576=DIRECTION('ref_axis',(0.585490553844361,0.810679228399879,0.));
#9577=DIRECTION('',(0.,0.,1.));
#9578=DIRECTION('',(-0.585490553844361,-0.810679228399879,0.));
#9579=DIRECTION('',(0.585490553844361,0.810679228399879,0.));
#9580=DIRECTION('center_axis',(0.810679228399883,0.585490553844356,0.));
#9581=DIRECTION('ref_axis',(0.585490553844356,-0.810679228399883,0.));
#9582=DIRECTION('',(0.,0.,-1.));
#9583=DIRECTION('',(0.585490553844356,-0.810679228399883,0.));
#9584=DIRECTION('',(0.,0.,-1.));
#9585=DIRECTION('',(-0.585490553844356,0.810679228399883,0.));
#9586=DIRECTION('center_axis',(-0.810679228399883,0.585490553844356,0.));
#9587=DIRECTION('ref_axis',(0.585490553844356,0.810679228399883,0.));
#9588=DIRECTION('',(0.,0.,1.));
#9589=DIRECTION('',(-0.585490553844356,-0.810679228399883,0.));
#9590=DIRECTION('',(0.585490553844356,0.810679228399883,0.));
#9591=DIRECTION('center_axis',(0.810679228399879,0.585490553844361,0.));
#9592=DIRECTION('ref_axis',(0.585490553844361,-0.810679228399879,0.));
#9593=DIRECTION('',(0.,0.,-1.));
#9594=DIRECTION('',(0.585490553844361,-0.810679228399879,0.));
#9595=DIRECTION('',(0.,0.,-1.));
#9596=DIRECTION('',(-0.585490553844361,0.810679228399879,0.));
#9597=DIRECTION('center_axis',(-0.810679228399883,0.585490553844356,0.));
#9598=DIRECTION('ref_axis',(0.585490553844356,0.810679228399883,0.));
#9599=DIRECTION('',(0.,0.,1.));
#9600=DIRECTION('',(-0.585490553844356,-0.810679228399883,0.));
#9601=DIRECTION('',(0.585490553844356,0.810679228399883,0.));
#9602=DIRECTION('center_axis',(0.810679228399883,0.585490553844356,0.));
#9603=DIRECTION('ref_axis',(0.585490553844356,-0.810679228399883,0.));
#9604=DIRECTION('',(0.,0.,-1.));
#9605=DIRECTION('',(0.585490553844356,-0.810679228399883,0.));
#9606=DIRECTION('',(0.,0.,-1.));
#9607=DIRECTION('',(-0.585490553844356,0.810679228399883,0.));
#9608=DIRECTION('center_axis',(-0.810679228399879,0.585490553844361,0.));
#9609=DIRECTION('ref_axis',(0.585490553844361,0.810679228399879,0.));
#9610=DIRECTION('',(0.,0.,1.));
#9611=DIRECTION('',(-0.585490553844361,-0.810679228399879,0.));
#9612=DIRECTION('',(0.585490553844361,0.810679228399879,0.));
#9613=DIRECTION('center_axis',(0.810679228399879,0.585490553844361,0.));
#9614=DIRECTION('ref_axis',(0.585490553844361,-0.810679228399879,0.));
#9615=DIRECTION('',(0.,0.,-1.));
#9616=DIRECTION('',(0.585490553844361,-0.810679228399879,0.));
#9617=DIRECTION('',(0.,0.,-1.));
#9618=DIRECTION('',(-0.585490553844361,0.810679228399879,0.));
#9619=DIRECTION('center_axis',(-0.810679228399883,0.585490553844356,0.));
#9620=DIRECTION('ref_axis',(0.585490553844356,0.810679228399883,0.));
#9621=DIRECTION('',(0.,0.,1.));
#9622=DIRECTION('',(-0.585490553844356,-0.810679228399883,0.));
#9623=DIRECTION('',(0.585490553844356,0.810679228399883,0.));
#9624=DIRECTION('center_axis',(0.810679228399883,0.585490553844356,0.));
#9625=DIRECTION('ref_axis',(0.585490553844356,-0.810679228399883,0.));
#9626=DIRECTION('',(0.,0.,-1.));
#9627=DIRECTION('',(0.585490553844356,-0.810679228399883,0.));
#9628=DIRECTION('',(0.,0.,-1.));
#9629=DIRECTION('',(-0.585490553844356,0.810679228399883,0.));
#9630=DIRECTION('center_axis',(-0.810679228399875,0.585490553844366,0.));
#9631=DIRECTION('ref_axis',(0.585490553844366,0.810679228399875,0.));
#9632=DIRECTION('',(0.,0.,1.));
#9633=DIRECTION('',(-0.585490553844366,-0.810679228399875,0.));
#9634=DIRECTION('',(0.585490553844366,0.810679228399875,0.));
#9635=DIRECTION('center_axis',(0.810679228399879,0.585490553844361,0.));
#9636=DIRECTION('ref_axis',(0.585490553844361,-0.810679228399879,0.));
#9637=DIRECTION('',(0.,0.,-1.));
#9638=DIRECTION('',(0.585490553844361,-0.810679228399879,0.));
#9639=DIRECTION('',(0.,0.,-1.));
#9640=DIRECTION('',(-0.585490553844361,0.810679228399879,0.));
#9641=DIRECTION('center_axis',(-0.810679228399879,0.585490553844361,0.));
#9642=DIRECTION('ref_axis',(0.585490553844361,0.810679228399879,0.));
#9643=DIRECTION('',(0.,0.,1.));
#9644=DIRECTION('',(-0.585490553844361,-0.810679228399879,0.));
#9645=DIRECTION('',(0.585490553844361,0.810679228399879,0.));
#9646=DIRECTION('center_axis',(0.810679228399879,0.585490553844361,0.));
#9647=DIRECTION('ref_axis',(0.585490553844361,-0.810679228399879,0.));
#9648=DIRECTION('',(0.,0.,-1.));
#9649=DIRECTION('',(0.585490553844361,-0.810679228399879,0.));
#9650=DIRECTION('',(0.,0.,-1.));
#9651=DIRECTION('',(-0.585490553844361,0.810679228399879,0.));
#9652=DIRECTION('center_axis',(-0.810679228399879,0.585490553844361,0.));
#9653=DIRECTION('ref_axis',(0.585490553844361,0.810679228399879,0.));
#9654=DIRECTION('',(0.,0.,1.));
#9655=DIRECTION('',(-0.585490553844361,-0.810679228399879,0.));
#9656=DIRECTION('',(0.585490553844361,0.810679228399879,0.));
#9657=DIRECTION('center_axis',(0.810679228399879,0.585490553844361,0.));
#9658=DIRECTION('ref_axis',(0.585490553844361,-0.810679228399879,0.));
#9659=DIRECTION('',(0.,0.,-1.));
#9660=DIRECTION('',(0.585490553844361,-0.810679228399879,0.));
#9661=DIRECTION('',(0.,0.,-1.));
#9662=DIRECTION('',(-0.585490553844361,0.810679228399879,0.));
#9663=DIRECTION('center_axis',(-0.810679228399875,0.585490553844366,0.));
#9664=DIRECTION('ref_axis',(0.585490553844366,0.810679228399875,0.));
#9665=DIRECTION('',(0.,0.,1.));
#9666=DIRECTION('',(-0.585490553844366,-0.810679228399875,0.));
#9667=DIRECTION('',(0.585490553844366,0.810679228399875,0.));
#9668=DIRECTION('center_axis',(0.810679228399879,0.585490553844361,0.));
#9669=DIRECTION('ref_axis',(0.585490553844361,-0.810679228399879,0.));
#9670=DIRECTION('',(0.,0.,-1.));
#9671=DIRECTION('',(0.585490553844361,-0.810679228399879,0.));
#9672=DIRECTION('',(0.,0.,-1.));
#9673=DIRECTION('',(-0.585490553844361,0.810679228399879,0.));
#9674=DIRECTION('center_axis',(-0.810679228399875,0.585490553844366,0.));
#9675=DIRECTION('ref_axis',(0.585490553844366,0.810679228399875,0.));
#9676=DIRECTION('',(0.,0.,1.));
#9677=DIRECTION('',(-0.585490553844366,-0.810679228399875,0.));
#9678=DIRECTION('',(0.585490553844366,0.810679228399875,0.));
#9679=DIRECTION('center_axis',(0.810679228399875,0.585490553844366,0.));
#9680=DIRECTION('ref_axis',(0.585490553844366,-0.810679228399875,0.));
#9681=DIRECTION('',(0.,0.,-1.));
#9682=DIRECTION('',(0.585490553844366,-0.810679228399875,0.));
#9683=DIRECTION('',(0.,0.,-1.));
#9684=DIRECTION('',(-0.585490553844366,0.810679228399875,0.));
#9685=DIRECTION('center_axis',(-0.810679228399883,0.585490553844356,0.));
#9686=DIRECTION('ref_axis',(0.585490553844356,0.810679228399883,0.));
#9687=DIRECTION('',(0.,0.,1.));
#9688=DIRECTION('',(-0.585490553844356,-0.810679228399883,0.));
#9689=DIRECTION('',(0.585490553844356,0.810679228399883,0.));
#9690=DIRECTION('center_axis',(0.810679228399875,0.585490553844366,0.));
#9691=DIRECTION('ref_axis',(0.585490553844366,-0.810679228399875,0.));
#9692=DIRECTION('',(0.,0.,-1.));
#9693=DIRECTION('',(0.585490553844366,-0.810679228399875,0.));
#9694=DIRECTION('',(0.,0.,-1.));
#9695=DIRECTION('',(-0.585490553844366,0.810679228399875,0.));
#9696=DIRECTION('center_axis',(-0.810679228399883,0.585490553844356,0.));
#9697=DIRECTION('ref_axis',(0.585490553844356,0.810679228399883,0.));
#9698=DIRECTION('',(0.,0.,1.));
#9699=DIRECTION('',(-0.585490553844356,-0.810679228399883,0.));
#9700=DIRECTION('',(0.585490553844356,0.810679228399883,0.));
#9701=DIRECTION('center_axis',(0.810679228399883,0.585490553844356,0.));
#9702=DIRECTION('ref_axis',(0.585490553844356,-0.810679228399883,0.));
#9703=DIRECTION('',(0.,0.,-1.));
#9704=DIRECTION('',(0.585490553844356,-0.810679228399883,0.));
#9705=DIRECTION('',(0.,0.,-1.));
#9706=DIRECTION('',(-0.585490553844356,0.810679228399883,0.));
#9707=DIRECTION('center_axis',(-0.810679228399875,0.585490553844366,0.));
#9708=DIRECTION('ref_axis',(0.585490553844366,0.810679228399875,0.));
#9709=DIRECTION('',(0.,0.,1.));
#9710=DIRECTION('',(-0.585490553844366,-0.810679228399875,0.));
#9711=DIRECTION('',(0.585490553844366,0.810679228399875,0.));
#9712=DIRECTION('center_axis',(0.810679228399883,0.585490553844356,0.));
#9713=DIRECTION('ref_axis',(0.585490553844356,-0.810679228399883,0.));
#9714=DIRECTION('',(0.,0.,-1.));
#9715=DIRECTION('',(0.585490553844356,-0.810679228399883,0.));
#9716=DIRECTION('',(0.,0.,-1.));
#9717=DIRECTION('',(-0.585490553844356,0.810679228399883,0.));
#9718=DIRECTION('center_axis',(-0.810679228399875,0.585490553844366,0.));
#9719=DIRECTION('ref_axis',(0.585490553844366,0.810679228399875,0.));
#9720=DIRECTION('',(0.,0.,1.));
#9721=DIRECTION('',(-0.585490553844366,-0.810679228399875,0.));
#9722=DIRECTION('',(0.585490553844366,0.810679228399875,0.));
#9723=DIRECTION('center_axis',(0.810679228399875,0.585490553844366,0.));
#9724=DIRECTION('ref_axis',(0.585490553844366,-0.810679228399875,0.));
#9725=DIRECTION('',(0.,0.,-1.));
#9726=DIRECTION('',(0.585490553844366,-0.810679228399875,0.));
#9727=DIRECTION('',(0.,0.,-1.));
#9728=DIRECTION('',(-0.585490553844366,0.810679228399875,0.));
#9729=DIRECTION('center_axis',(-0.810679228399875,0.585490553844366,0.));
#9730=DIRECTION('ref_axis',(0.585490553844366,0.810679228399875,0.));
#9731=DIRECTION('',(0.,0.,1.));
#9732=DIRECTION('',(-0.585490553844366,-0.810679228399875,0.));
#9733=DIRECTION('',(0.585490553844366,0.810679228399875,0.));
#9734=DIRECTION('center_axis',(0.810679228399875,0.585490553844366,0.));
#9735=DIRECTION('ref_axis',(0.585490553844366,-0.810679228399875,0.));
#9736=DIRECTION('',(0.,0.,-1.));
#9737=DIRECTION('',(0.585490553844366,-0.810679228399875,0.));
#9738=DIRECTION('',(0.,0.,-1.));
#9739=DIRECTION('',(-0.585490553844366,0.810679228399875,0.));
#9740=DIRECTION('center_axis',(-0.810679228399883,0.585490553844356,0.));
#9741=DIRECTION('ref_axis',(0.585490553844356,0.810679228399883,0.));
#9742=DIRECTION('',(0.,0.,1.));
#9743=DIRECTION('',(-0.585490553844356,-0.810679228399883,0.));
#9744=DIRECTION('',(0.585490553844356,0.810679228399883,0.));
#9745=DIRECTION('center_axis',(0.810679228399875,0.585490553844366,0.));
#9746=DIRECTION('ref_axis',(0.585490553844366,-0.810679228399875,0.));
#9747=DIRECTION('',(0.,0.,-1.));
#9748=DIRECTION('',(0.585490553844366,-0.810679228399875,0.));
#9749=DIRECTION('',(0.,0.,-1.));
#9750=DIRECTION('',(-0.585490553844366,0.810679228399875,0.));
#9751=DIRECTION('center_axis',(-0.810679228399883,0.585490553844356,0.));
#9752=DIRECTION('ref_axis',(0.585490553844356,0.810679228399883,0.));
#9753=DIRECTION('',(0.,0.,1.));
#9754=DIRECTION('',(-0.585490553844356,-0.810679228399883,0.));
#9755=DIRECTION('',(0.585490553844356,0.810679228399883,0.));
#9756=DIRECTION('center_axis',(0.810679228399875,0.585490553844366,0.));
#9757=DIRECTION('ref_axis',(0.585490553844366,-0.810679228399875,0.));
#9758=DIRECTION('',(0.,0.,-1.));
#9759=DIRECTION('',(0.585490553844366,-0.810679228399875,0.));
#9760=DIRECTION('',(0.,0.,-1.));
#9761=DIRECTION('',(-0.585490553844366,0.810679228399875,0.));
#9762=DIRECTION('center_axis',(-0.810679228399875,0.585490553844366,0.));
#9763=DIRECTION('ref_axis',(0.585490553844366,0.810679228399875,0.));
#9764=DIRECTION('',(0.,0.,1.));
#9765=DIRECTION('',(-0.585490553844366,-0.810679228399875,0.));
#9766=DIRECTION('',(0.585490553844366,0.810679228399875,0.));
#9767=DIRECTION('center_axis',(0.810679228399883,0.585490553844356,0.));
#9768=DIRECTION('ref_axis',(0.585490553844356,-0.810679228399883,0.));
#9769=DIRECTION('',(0.,0.,-1.));
#9770=DIRECTION('',(0.585490553844356,-0.810679228399883,0.));
#9771=DIRECTION('',(0.,0.,-1.));
#9772=DIRECTION('',(-0.585490553844356,0.810679228399883,0.));
#9773=DIRECTION('center_axis',(-0.810679228399875,0.585490553844366,0.));
#9774=DIRECTION('ref_axis',(0.585490553844366,0.810679228399875,0.));
#9775=DIRECTION('',(0.,0.,1.));
#9776=DIRECTION('',(-0.585490553844366,-0.810679228399875,0.));
#9777=DIRECTION('',(0.585490553844366,0.810679228399875,0.));
#9778=DIRECTION('center_axis',(0.810679228399883,0.585490553844356,0.));
#9779=DIRECTION('ref_axis',(0.585490553844356,-0.810679228399883,0.));
#9780=DIRECTION('',(0.,0.,-1.));
#9781=DIRECTION('',(0.585490553844356,-0.810679228399883,0.));
#9782=DIRECTION('',(0.,0.,-1.));
#9783=DIRECTION('',(-0.585490553844356,0.810679228399883,0.));
#9784=DIRECTION('center_axis',(-0.810679228399875,0.585490553844366,0.));
#9785=DIRECTION('ref_axis',(0.585490553844366,0.810679228399875,0.));
#9786=DIRECTION('',(0.,0.,1.));
#9787=DIRECTION('',(-0.585490553844366,-0.810679228399875,0.));
#9788=DIRECTION('',(0.585490553844366,0.810679228399875,0.));
#9789=DIRECTION('center_axis',(0.810679228399879,0.585490553844361,0.));
#9790=DIRECTION('ref_axis',(0.585490553844361,-0.810679228399879,0.));
#9791=DIRECTION('',(0.,0.,-1.));
#9792=DIRECTION('',(0.585490553844361,-0.810679228399879,0.));
#9793=DIRECTION('',(0.,0.,-1.));
#9794=DIRECTION('',(-0.585490553844361,0.810679228399879,0.));
#9795=DIRECTION('center_axis',(-0.810679228399879,0.585490553844361,0.));
#9796=DIRECTION('ref_axis',(0.585490553844361,0.810679228399879,0.));
#9797=DIRECTION('',(0.,0.,1.));
#9798=DIRECTION('',(-0.585490553844361,-0.810679228399879,0.));
#9799=DIRECTION('',(0.585490553844361,0.810679228399879,0.));
#9800=DIRECTION('center_axis',(0.810679228399875,0.585490553844366,0.));
#9801=DIRECTION('ref_axis',(0.585490553844366,-0.810679228399875,0.));
#9802=DIRECTION('',(0.,0.,-1.));
#9803=DIRECTION('',(0.585490553844366,-0.810679228399875,0.));
#9804=DIRECTION('',(0.,0.,-1.));
#9805=DIRECTION('',(-0.585490553844366,0.810679228399875,0.));
#9806=DIRECTION('center_axis',(-0.810679228399879,0.585490553844361,0.));
#9807=DIRECTION('ref_axis',(0.585490553844361,0.810679228399879,0.));
#9808=DIRECTION('',(0.,0.,1.));
#9809=DIRECTION('',(-0.585490553844361,-0.810679228399879,0.));
#9810=DIRECTION('',(0.585490553844361,0.810679228399879,0.));
#9811=DIRECTION('center_axis',(0.810679228399879,0.585490553844361,0.));
#9812=DIRECTION('ref_axis',(0.585490553844361,-0.810679228399879,0.));
#9813=DIRECTION('',(0.,0.,-1.));
#9814=DIRECTION('',(0.585490553844361,-0.810679228399879,0.));
#9815=DIRECTION('',(0.,0.,-1.));
#9816=DIRECTION('',(-0.585490553844361,0.810679228399879,0.));
#9817=DIRECTION('center_axis',(-0.810679228399879,0.585490553844361,0.));
#9818=DIRECTION('ref_axis',(0.585490553844361,0.810679228399879,0.));
#9819=DIRECTION('',(0.,0.,1.));
#9820=DIRECTION('',(-0.585490553844361,-0.810679228399879,0.));
#9821=DIRECTION('',(0.585490553844361,0.810679228399879,0.));
#9822=DIRECTION('center_axis',(0.810679228399879,0.585490553844361,0.));
#9823=DIRECTION('ref_axis',(0.585490553844361,-0.810679228399879,0.));
#9824=DIRECTION('',(0.,0.,-1.));
#9825=DIRECTION('',(0.585490553844361,-0.810679228399879,0.));
#9826=DIRECTION('',(0.,0.,-1.));
#9827=DIRECTION('',(-0.585490553844361,0.810679228399879,0.));
#9828=DIRECTION('center_axis',(-0.810679228399875,0.585490553844366,0.));
#9829=DIRECTION('ref_axis',(0.585490553844366,0.810679228399875,0.));
#9830=DIRECTION('',(0.,0.,1.));
#9831=DIRECTION('',(-0.585490553844366,-0.810679228399875,0.));
#9832=DIRECTION('',(0.585490553844366,0.810679228399875,0.));
#9833=DIRECTION('center_axis',(0.810679228399879,0.585490553844361,0.));
#9834=DIRECTION('ref_axis',(0.585490553844361,-0.810679228399879,0.));
#9835=DIRECTION('',(0.,0.,-1.));
#9836=DIRECTION('',(0.585490553844361,-0.810679228399879,0.));
#9837=DIRECTION('',(0.,0.,-1.));
#9838=DIRECTION('',(-0.585490553844361,0.810679228399879,0.));
#9839=DIRECTION('center_axis',(-0.810679228399879,0.585490553844361,0.));
#9840=DIRECTION('ref_axis',(0.585490553844361,0.810679228399879,0.));
#9841=DIRECTION('',(0.,0.,1.));
#9842=DIRECTION('',(-0.585490553844361,-0.810679228399879,0.));
#9843=DIRECTION('',(0.585490553844361,0.810679228399879,0.));
#9844=DIRECTION('center_axis',(0.810679228399883,0.585490553844356,0.));
#9845=DIRECTION('ref_axis',(0.585490553844356,-0.810679228399883,0.));
#9846=DIRECTION('',(0.,0.,-1.));
#9847=DIRECTION('',(0.585490553844356,-0.810679228399883,0.));
#9848=DIRECTION('',(0.,0.,-1.));
#9849=DIRECTION('',(-0.585490553844356,0.810679228399883,0.));
#9850=DIRECTION('center_axis',(-0.810679228399883,0.585490553844356,0.));
#9851=DIRECTION('ref_axis',(0.585490553844356,0.810679228399883,0.));
#9852=DIRECTION('',(0.,0.,1.));
#9853=DIRECTION('',(-0.585490553844356,-0.810679228399883,0.));
#9854=DIRECTION('',(0.585490553844356,0.810679228399883,0.));
#9855=DIRECTION('center_axis',(0.810679228399883,0.585490553844356,0.));
#9856=DIRECTION('ref_axis',(0.585490553844356,-0.810679228399883,0.));
#9857=DIRECTION('',(0.,0.,-1.));
#9858=DIRECTION('',(0.585490553844356,-0.810679228399883,0.));
#9859=DIRECTION('',(0.,0.,-1.));
#9860=DIRECTION('',(-0.585490553844356,0.810679228399883,0.));
#9861=DIRECTION('center_axis',(-0.810679228399879,0.585490553844361,0.));
#9862=DIRECTION('ref_axis',(0.585490553844361,0.810679228399879,0.));
#9863=DIRECTION('',(0.,0.,1.));
#9864=DIRECTION('',(-0.585490553844361,-0.810679228399879,0.));
#9865=DIRECTION('',(0.585490553844361,0.810679228399879,0.));
#9866=DIRECTION('center_axis',(0.810679228399879,0.585490553844361,0.));
#9867=DIRECTION('ref_axis',(0.585490553844361,-0.810679228399879,0.));
#9868=DIRECTION('',(0.,0.,-1.));
#9869=DIRECTION('',(0.585490553844361,-0.810679228399879,0.));
#9870=DIRECTION('',(0.,0.,-1.));
#9871=DIRECTION('',(-0.585490553844361,0.810679228399879,0.));
#9872=DIRECTION('center_axis',(-0.810679228399883,0.585490553844356,0.));
#9873=DIRECTION('ref_axis',(0.585490553844356,0.810679228399883,0.));
#9874=DIRECTION('',(0.,0.,1.));
#9875=DIRECTION('',(-0.585490553844356,-0.810679228399883,0.));
#9876=DIRECTION('',(0.585490553844356,0.810679228399883,0.));
#9877=DIRECTION('center_axis',(0.810679228399883,0.585490553844356,0.));
#9878=DIRECTION('ref_axis',(0.585490553844356,-0.810679228399883,0.));
#9879=DIRECTION('',(0.,0.,-1.));
#9880=DIRECTION('',(0.585490553844356,-0.810679228399883,0.));
#9881=DIRECTION('',(0.,0.,-1.));
#9882=DIRECTION('',(-0.585490553844356,0.810679228399883,0.));
#9883=DIRECTION('center_axis',(-0.810679228399879,0.585490553844361,0.));
#9884=DIRECTION('ref_axis',(0.585490553844361,0.810679228399879,0.));
#9885=DIRECTION('',(0.,0.,1.));
#9886=DIRECTION('',(-0.585490553844361,-0.810679228399879,0.));
#9887=DIRECTION('',(0.585490553844361,0.810679228399879,0.));
#9888=DIRECTION('center_axis',(0.810679228399879,0.585490553844361,0.));
#9889=DIRECTION('ref_axis',(0.585490553844361,-0.810679228399879,0.));
#9890=DIRECTION('',(0.,0.,-1.));
#9891=DIRECTION('',(0.585490553844361,-0.810679228399879,0.));
#9892=DIRECTION('',(0.,0.,-1.));
#9893=DIRECTION('',(-0.585490553844361,0.810679228399879,0.));
#9894=DIRECTION('center_axis',(-0.810679228399883,0.585490553844356,0.));
#9895=DIRECTION('ref_axis',(0.585490553844356,0.810679228399883,0.));
#9896=DIRECTION('',(0.,0.,1.));
#9897=DIRECTION('',(-0.585490553844356,-0.810679228399883,0.));
#9898=DIRECTION('',(0.585490553844356,0.810679228399883,0.));
#9899=DIRECTION('center_axis',(0.810679228399881,0.585490553844358,0.));
#9900=DIRECTION('ref_axis',(0.585490553844358,-0.810679228399881,0.));
#9901=DIRECTION('',(0.,0.,-1.));
#9902=DIRECTION('',(0.585490553844358,-0.810679228399881,0.));
#9903=DIRECTION('',(0.,0.,-1.));
#9904=DIRECTION('',(-0.585490553844358,0.810679228399881,0.));
#9905=DIRECTION('center_axis',(-0.810679228399883,0.585490553844356,0.));
#9906=DIRECTION('ref_axis',(0.585490553844356,0.810679228399883,0.));
#9907=DIRECTION('',(0.,0.,1.));
#9908=DIRECTION('',(-0.585490553844356,-0.810679228399883,0.));
#9909=DIRECTION('',(0.585490553844356,0.810679228399883,0.));
#9910=DIRECTION('center_axis',(0.810679228399881,0.585490553844358,0.));
#9911=DIRECTION('ref_axis',(0.585490553844358,-0.810679228399881,0.));
#9912=DIRECTION('',(0.,0.,-1.));
#9913=DIRECTION('',(0.585490553844358,-0.810679228399881,0.));
#9914=DIRECTION('',(0.,0.,-1.));
#9915=DIRECTION('',(-0.585490553844358,0.810679228399881,0.));
#9916=DIRECTION('center_axis',(-0.810679228399881,0.585490553844358,0.));
#9917=DIRECTION('ref_axis',(0.585490553844358,0.810679228399881,0.));
#9918=DIRECTION('',(0.,0.,1.));
#9919=DIRECTION('',(-0.585490553844358,-0.810679228399881,0.));
#9920=DIRECTION('',(0.585490553844358,0.810679228399881,0.));
#9921=DIRECTION('center_axis',(0.810679228399881,0.585490553844358,0.));
#9922=DIRECTION('ref_axis',(0.585490553844358,-0.810679228399881,0.));
#9923=DIRECTION('',(0.,0.,-1.));
#9924=DIRECTION('',(0.585490553844358,-0.810679228399881,0.));
#9925=DIRECTION('',(0.,0.,-1.));
#9926=DIRECTION('',(-0.585490553844358,0.810679228399881,0.));
#9927=DIRECTION('center_axis',(-0.810679228399883,0.585490553844356,0.));
#9928=DIRECTION('ref_axis',(0.585490553844356,0.810679228399883,0.));
#9929=DIRECTION('',(0.,0.,1.));
#9930=DIRECTION('',(-0.585490553844356,-0.810679228399883,0.));
#9931=DIRECTION('',(0.585490553844356,0.810679228399883,0.));
#9932=DIRECTION('center_axis',(0.810679228399883,0.585490553844356,0.));
#9933=DIRECTION('ref_axis',(0.585490553844356,-0.810679228399883,0.));
#9934=DIRECTION('',(0.,0.,-1.));
#9935=DIRECTION('',(0.585490553844356,-0.810679228399883,0.));
#9936=DIRECTION('',(0.,0.,-1.));
#9937=DIRECTION('',(-0.585490553844356,0.810679228399883,0.));
#9938=DIRECTION('center_axis',(-0.810679228399881,0.585490553844358,0.));
#9939=DIRECTION('ref_axis',(0.585490553844358,0.810679228399881,0.));
#9940=DIRECTION('',(0.,0.,1.));
#9941=DIRECTION('',(-0.585490553844358,-0.810679228399881,0.));
#9942=DIRECTION('',(0.585490553844358,0.810679228399881,0.));
#9943=DIRECTION('center_axis',(0.,-1.,0.));
#9944=DIRECTION('ref_axis',(1.,0.,0.));
#9945=DIRECTION('',(-1.,0.,0.));
#9946=DIRECTION('',(0.,0.,1.));
#9947=DIRECTION('',(-1.,0.,0.));
#9948=DIRECTION('',(0.,0.,-1.));
#9949=DIRECTION('',(1.,0.,0.));
#9950=DIRECTION('center_axis',(0.,-1.,0.));
#9951=DIRECTION('ref_axis',(1.,0.,0.));
#9952=DIRECTION('',(-1.,0.,0.));
#9953=DIRECTION('',(1.,0.,0.));
#9954=DIRECTION('center_axis',(0.,-1.,0.));
#9955=DIRECTION('ref_axis',(1.,0.,0.));
#9956=DIRECTION('',(-1.,0.,0.));
#9957=DIRECTION('',(1.,0.,0.));
#9958=DIRECTION('center_axis',(0.,-1.,0.));
#9959=DIRECTION('ref_axis',(1.,0.,0.));
#9960=DIRECTION('',(-1.,0.,0.));
#9961=DIRECTION('',(1.,0.,0.));
#9962=DIRECTION('center_axis',(0.,-1.,0.));
#9963=DIRECTION('ref_axis',(1.,0.,0.));
#9964=DIRECTION('',(-1.,0.,0.));
#9965=DIRECTION('',(1.,0.,0.));
#9966=DIRECTION('center_axis',(0.,-1.,0.));
#9967=DIRECTION('ref_axis',(1.,0.,0.));
#9968=DIRECTION('',(-1.,0.,0.));
#9969=DIRECTION('',(1.,0.,0.));
#9970=DIRECTION('center_axis',(0.,-1.,0.));
#9971=DIRECTION('ref_axis',(1.,0.,0.));
#9972=DIRECTION('',(-1.,0.,0.));
#9973=DIRECTION('',(1.,0.,0.));
#9974=DIRECTION('center_axis',(0.,-1.,0.));
#9975=DIRECTION('ref_axis',(1.,0.,0.));
#9976=DIRECTION('',(-1.,0.,0.));
#9977=DIRECTION('',(1.,0.,0.));
#9978=DIRECTION('center_axis',(0.,-1.,0.));
#9979=DIRECTION('ref_axis',(1.,0.,0.));
#9980=DIRECTION('',(-1.,0.,0.));
#9981=DIRECTION('',(1.,0.,0.));
#9982=DIRECTION('center_axis',(0.,-1.,0.));
#9983=DIRECTION('ref_axis',(1.,0.,0.));
#9984=DIRECTION('',(-1.,0.,0.));
#9985=DIRECTION('',(1.,0.,0.));
#9986=DIRECTION('center_axis',(0.,-1.,0.));
#9987=DIRECTION('ref_axis',(1.,0.,0.));
#9988=DIRECTION('',(-1.,0.,0.));
#9989=DIRECTION('',(1.,0.,0.));
#9990=DIRECTION('center_axis',(0.,-1.,0.));
#9991=DIRECTION('ref_axis',(1.,0.,0.));
#9992=DIRECTION('',(-1.,0.,0.));
#9993=DIRECTION('',(1.,0.,0.));
#9994=DIRECTION('center_axis',(0.,-1.,0.));
#9995=DIRECTION('ref_axis',(1.,0.,0.));
#9996=DIRECTION('',(-1.,0.,0.));
#9997=DIRECTION('',(1.,0.,0.));
#9998=DIRECTION('center_axis',(0.,-1.,0.));
#9999=DIRECTION('ref_axis',(1.,0.,0.));
#10000=DIRECTION('',(-1.,0.,0.));
#10001=DIRECTION('',(1.,0.,0.));
#10002=DIRECTION('center_axis',(0.,-1.,0.));
#10003=DIRECTION('ref_axis',(1.,0.,0.));
#10004=DIRECTION('',(-1.,0.,0.));
#10005=DIRECTION('',(1.,0.,0.));
#10006=DIRECTION('center_axis',(0.,-1.,0.));
#10007=DIRECTION('ref_axis',(1.,0.,0.));
#10008=DIRECTION('',(-1.,0.,0.));
#10009=DIRECTION('',(1.,0.,0.));
#10010=DIRECTION('center_axis',(0.,-1.,0.));
#10011=DIRECTION('ref_axis',(1.,0.,0.));
#10012=DIRECTION('',(-1.,0.,0.));
#10013=DIRECTION('',(1.,0.,0.));
#10014=DIRECTION('center_axis',(0.,-1.,0.));
#10015=DIRECTION('ref_axis',(1.,0.,0.));
#10016=DIRECTION('',(-1.,0.,0.));
#10017=DIRECTION('',(1.,0.,0.));
#10018=DIRECTION('center_axis',(0.,-1.,0.));
#10019=DIRECTION('ref_axis',(1.,0.,0.));
#10020=DIRECTION('',(-1.,0.,0.));
#10021=DIRECTION('',(1.,0.,0.));
#10022=DIRECTION('center_axis',(0.,-1.,0.));
#10023=DIRECTION('ref_axis',(1.,0.,0.));
#10024=DIRECTION('',(-1.,0.,0.));
#10025=DIRECTION('',(1.,0.,0.));
#10026=DIRECTION('center_axis',(0.,-1.,0.));
#10027=DIRECTION('ref_axis',(1.,0.,0.));
#10028=DIRECTION('',(-1.,0.,0.));
#10029=DIRECTION('',(1.,0.,0.));
#10030=DIRECTION('center_axis',(0.,-1.,0.));
#10031=DIRECTION('ref_axis',(1.,0.,0.));
#10032=DIRECTION('',(1.,0.,0.));
#10033=DIRECTION('',(-1.,0.,0.));
#10034=DIRECTION('center_axis',(0.,-1.,0.));
#10035=DIRECTION('ref_axis',(1.,0.,0.));
#10036=DIRECTION('',(1.,0.,0.));
#10037=DIRECTION('',(-1.,0.,0.));
#10038=DIRECTION('center_axis',(0.,-1.,0.));
#10039=DIRECTION('ref_axis',(1.,0.,0.));
#10040=DIRECTION('',(1.,0.,0.));
#10041=DIRECTION('',(-1.,0.,0.));
#10042=DIRECTION('center_axis',(0.,-1.,0.));
#10043=DIRECTION('ref_axis',(1.,0.,0.));
#10044=DIRECTION('',(1.,0.,0.));
#10045=DIRECTION('',(-1.,0.,0.));
#10046=DIRECTION('center_axis',(0.,-1.,0.));
#10047=DIRECTION('ref_axis',(1.,0.,0.));
#10048=DIRECTION('',(1.,0.,0.));
#10049=DIRECTION('',(-1.,0.,0.));
#10050=DIRECTION('center_axis',(0.,-1.,0.));
#10051=DIRECTION('ref_axis',(1.,0.,0.));
#10052=DIRECTION('',(1.,0.,0.));
#10053=DIRECTION('',(-1.,0.,0.));
#10054=DIRECTION('center_axis',(0.,-1.,0.));
#10055=DIRECTION('ref_axis',(1.,0.,0.));
#10056=DIRECTION('',(1.,0.,0.));
#10057=DIRECTION('',(-1.,0.,0.));
#10058=DIRECTION('center_axis',(0.,-1.,0.));
#10059=DIRECTION('ref_axis',(1.,0.,0.));
#10060=DIRECTION('',(1.,0.,0.));
#10061=DIRECTION('',(-1.,0.,0.));
#10062=DIRECTION('center_axis',(0.,-1.,0.));
#10063=DIRECTION('ref_axis',(1.,0.,0.));
#10064=DIRECTION('',(1.,0.,0.));
#10065=DIRECTION('',(0.,0.,1.));
#10066=DIRECTION('',(-1.,0.,0.));
#10067=DIRECTION('center_axis',(0.,-1.,0.));
#10068=DIRECTION('ref_axis',(1.,0.,0.));
#10069=DIRECTION('',(1.,0.,0.));
#10070=DIRECTION('',(-1.,0.,0.));
#10071=DIRECTION('center_axis',(0.,-1.,0.));
#10072=DIRECTION('ref_axis',(1.,0.,0.));
#10073=DIRECTION('',(1.,0.,0.));
#10074=DIRECTION('',(-1.,0.,0.));
#10075=DIRECTION('center_axis',(0.,-1.,0.));
#10076=DIRECTION('ref_axis',(1.,0.,0.));
#10077=DIRECTION('',(1.,0.,0.));
#10078=DIRECTION('',(-1.,0.,0.));
#10079=DIRECTION('center_axis',(0.,-1.,0.));
#10080=DIRECTION('ref_axis',(1.,0.,0.));
#10081=DIRECTION('',(1.,0.,0.));
#10082=DIRECTION('',(-1.,0.,0.));
#10083=DIRECTION('center_axis',(0.,-1.,0.));
#10084=DIRECTION('ref_axis',(1.,0.,0.));
#10085=DIRECTION('',(1.,0.,0.));
#10086=DIRECTION('',(-1.,0.,0.));
#10087=DIRECTION('center_axis',(0.,-1.,0.));
#10088=DIRECTION('ref_axis',(1.,0.,0.));
#10089=DIRECTION('',(1.,0.,0.));
#10090=DIRECTION('',(-1.,0.,0.));
#10091=DIRECTION('center_axis',(0.,-1.,0.));
#10092=DIRECTION('ref_axis',(1.,0.,0.));
#10093=DIRECTION('',(1.,0.,0.));
#10094=DIRECTION('',(-1.,0.,0.));
#10095=DIRECTION('center_axis',(0.,-1.,0.));
#10096=DIRECTION('ref_axis',(1.,0.,0.));
#10097=DIRECTION('',(1.,0.,0.));
#10098=DIRECTION('',(-1.,0.,0.));
#10099=DIRECTION('center_axis',(0.,-1.,0.));
#10100=DIRECTION('ref_axis',(1.,0.,0.));
#10101=DIRECTION('',(1.,0.,0.));
#10102=DIRECTION('',(-1.,0.,0.));
#10103=DIRECTION('center_axis',(0.,0.,1.));
#10104=DIRECTION('ref_axis',(1.,0.,0.));
#10105=DIRECTION('',(0.,1.,0.));
#10106=DIRECTION('',(0.994646105081306,0.103339855073382,0.));
#10107=DIRECTION('',(1.,0.,0.));
#10108=DIRECTION('',(0.,-1.,0.));
#10109=DIRECTION('center_axis',(1.,0.,0.));
#10110=DIRECTION('ref_axis',(0.,1.,0.));
#10111=DIRECTION('',(0.,0.,1.));
#10112=DIRECTION('',(0.,1.,0.));
#10113=DIRECTION('center_axis',(1.,0.,0.));
#10114=DIRECTION('ref_axis',(0.,1.,0.));
#10115=DIRECTION('',(0.,0.,1.));
#10116=DIRECTION('',(0.,-1.,0.));
#10117=DIRECTION('',(0.,0.,1.));
#10118=DIRECTION('',(0.,1.,0.));
#10119=DIRECTION('center_axis',(-1.,0.,0.));
#10120=DIRECTION('ref_axis',(0.,-1.,0.));
#10121=DIRECTION('',(0.,-1.,0.));
#10122=DIRECTION('',(0.,0.,1.));
#10123=DIRECTION('center_axis',(-0.103339855073382,0.994646105081306,0.));
#10124=DIRECTION('ref_axis',(-0.994646105081306,-0.103339855073382,0.));
#10125=DIRECTION('',(-0.994646105081306,-0.103339855073382,0.));
#10126=DIRECTION('',(0.,0.,1.));
#10127=DIRECTION('center_axis',(0.,1.,0.));
#10128=DIRECTION('ref_axis',(-1.,0.,0.));
#10129=DIRECTION('',(-1.,0.,0.));
#10130=DIRECTION('',(1.,0.,0.));
#10131=DIRECTION('center_axis',(0.,0.,1.));
#10132=DIRECTION('ref_axis',(1.,0.,0.));
#10133=DIRECTION('center_axis',(0.,0.,1.));
#10134=DIRECTION('ref_axis',(1.,0.,0.));
#10135=DIRECTION('',(-0.447213595499958,-0.894427190999916,0.));
#10136=DIRECTION('',(-0.694594513699567,0.719401460617409,0.));
#10137=DIRECTION('',(-1.,0.,0.));
#10138=DIRECTION('',(0.,1.,0.));
#10139=DIRECTION('',(1.,0.,0.));
#10140=DIRECTION('',(0.87524153543927,-0.483686111690123,0.));
#10141=DIRECTION('center_axis',(0.,0.,1.));
#10142=DIRECTION('ref_axis',(1.,0.,0.));
#10143=DIRECTION('center_axis',(0.,0.,1.));
#10144=DIRECTION('ref_axis',(1.,0.,0.));
#10145=DIRECTION('center_axis',(0.,0.,1.));
#10146=DIRECTION('ref_axis',(1.,0.,0.));
#10147=DIRECTION('',(0.,0.,-1.));
#10148=DIRECTION('center_axis',(-0.483686111690123,-0.87524153543927,0.));
#10149=DIRECTION('ref_axis',(0.87524153543927,-0.483686111690123,0.));
#10150=DIRECTION('',(0.,0.,1.));
#10151=DIRECTION('',(0.,0.,1.));
#10152=DIRECTION('',(0.87524153543927,-0.483686111690123,0.));
#10153=DIRECTION('center_axis',(-0.894427190999916,0.447213595499958,0.));
#10154=DIRECTION('ref_axis',(-0.447213595499958,-0.894427190999916,0.));
#10155=DIRECTION('',(-0.447213595499958,-0.894427190999916,0.));
#10156=DIRECTION('',(0.,0.,1.));
#10157=DIRECTION('center_axis',(0.719401460617409,0.694594513699567,0.));
#10158=DIRECTION('ref_axis',(-0.694594513699567,0.719401460617409,0.));
#10159=DIRECTION('',(-0.694594513699567,0.719401460617409,0.));
#10160=DIRECTION('',(0.,0.,1.));
#10161=DIRECTION('center_axis',(0.,1.,0.));
#10162=DIRECTION('ref_axis',(-1.,0.,0.));
#10163=DIRECTION('',(-1.,0.,0.));
#10164=DIRECTION('',(0.,0.,1.));
#10165=DIRECTION('center_axis',(1.,0.,0.));
#10166=DIRECTION('ref_axis',(0.,1.,0.));
#10167=DIRECTION('',(0.,1.,0.));
#10168=DIRECTION('',(0.,0.,1.));
#10169=DIRECTION('center_axis',(0.,-1.,0.));
#10170=DIRECTION('ref_axis',(1.,0.,0.));
#10171=DIRECTION('',(1.,0.,0.));
#10172=DIRECTION('center_axis',(0.,0.,1.));
#10173=DIRECTION('ref_axis',(1.,0.,0.));
#10174=DIRECTION('center_axis',(0.,0.,1.));
#10175=DIRECTION('ref_axis',(1.,0.,0.));
#10176=DIRECTION('center_axis',(0.,0.,1.));
#10177=DIRECTION('ref_axis',(1.,0.,0.));
#10178=DIRECTION('axis',(0.,0.,1.));
#10179=DIRECTION('refdir',(1.,0.,0.));
#10180=DIRECTION('center_axis',(0.,0.,1.));
#10181=DIRECTION('ref_axis',(1.,0.,0.));
#10182=DIRECTION('center_axis',(0.,0.,1.));
#10183=DIRECTION('ref_axis',(1.,0.,0.));
#10184=DIRECTION('',(0.,0.,1.));
#10185=DIRECTION('center_axis',(0.,0.,1.));
#10186=DIRECTION('ref_axis',(1.,0.,0.));
#10187=DIRECTION('center_axis',(0.,0.,-1.));
#10188=DIRECTION('ref_axis',(-1.,0.,0.));
#10189=DIRECTION('center_axis',(0.,0.,-1.));
#10190=DIRECTION('ref_axis',(1.,0.,0.));
#10191=DIRECTION('center_axis',(0.,0.,1.));
#10192=DIRECTION('ref_axis',(1.,0.,0.));
#10193=DIRECTION('center_axis',(0.,0.,1.));
#10194=DIRECTION('ref_axis',(1.,0.,0.));
#10195=DIRECTION('center_axis',(0.,0.,1.));
#10196=DIRECTION('ref_axis',(1.,0.,0.));
#10197=DIRECTION('center_axis',(0.,0.,1.));
#10198=DIRECTION('ref_axis',(1.,0.,0.));
#10199=DIRECTION('',(0.,0.,-1.));
#10200=DIRECTION('center_axis',(0.,0.,1.));
#10201=DIRECTION('ref_axis',(1.,0.,0.));
#10202=DIRECTION('center_axis',(0.,0.,1.));
#10203=DIRECTION('ref_axis',(1.,0.,0.));
#10204=DIRECTION('center_axis',(0.,0.,1.));
#10205=DIRECTION('ref_axis',(1.,0.,0.));
#10206=DIRECTION('center_axis',(0.,0.,1.));
#10207=DIRECTION('ref_axis',(1.,0.,0.));
#10208=DIRECTION('',(0.,0.,-1.));
#10209=DIRECTION('center_axis',(0.,0.,1.));
#10210=DIRECTION('ref_axis',(1.,0.,0.));
#10211=DIRECTION('center_axis',(0.,0.,1.));
#10212=DIRECTION('ref_axis',(1.,0.,0.));
#10213=DIRECTION('center_axis',(0.,0.,1.));
#10214=DIRECTION('ref_axis',(1.,0.,0.));
#10215=DIRECTION('',(0.,0.,-1.));
#10216=DIRECTION('center_axis',(0.,0.,1.));
#10217=DIRECTION('ref_axis',(1.,0.,0.));
#10218=DIRECTION('axis',(0.,0.,1.));
#10219=DIRECTION('refdir',(1.,0.,0.));
#10220=DIRECTION('center_axis',(-1.,0.,0.));
#10221=DIRECTION('ref_axis',(0.,1.,0.));
#10222=DIRECTION('',(0.,0.,1.));
#10223=DIRECTION('',(0.,-1.,0.));
#10224=DIRECTION('',(0.,0.,-1.));
#10225=DIRECTION('',(0.,1.,0.));
#10226=DIRECTION('center_axis',(1.,0.,0.));
#10227=DIRECTION('ref_axis',(0.,-1.,0.));
#10228=DIRECTION('',(0.,0.,-1.));
#10229=DIRECTION('',(0.,-1.,0.));
#10230=DIRECTION('',(0.,0.,1.));
#10231=DIRECTION('',(0.,1.,0.));
#10232=DIRECTION('center_axis',(0.,0.,1.));
#10233=DIRECTION('ref_axis',(1.,0.,0.));
#10234=DIRECTION('center_axis',(0.,0.,1.));
#10235=DIRECTION('ref_axis',(1.,0.,0.));
#10236=DIRECTION('center_axis',(0.,0.,-1.));
#10237=DIRECTION('ref_axis',(1.,0.,0.));
#10238=DIRECTION('center_axis',(0.,0.,1.));
#10239=DIRECTION('ref_axis',(6.12323399573677E-17,-1.,0.));
#10240=DIRECTION('center_axis',(0.,0.,-1.));
#10241=DIRECTION('ref_axis',(1.,0.,0.));
#10242=DIRECTION('center_axis',(0.,0.,1.));
#10243=DIRECTION('ref_axis',(6.12323399573677E-17,-1.,0.));
#10244=DIRECTION('center_axis',(0.,0.,1.));
#10245=DIRECTION('ref_axis',(1.,0.,0.));
#10246=DIRECTION('center_axis',(0.,0.,1.));
#10247=DIRECTION('ref_axis',(1.,0.,0.));
#10248=DIRECTION('axis',(0.,0.,1.));
#10249=DIRECTION('refdir',(1.,0.,0.));
#10250=DIRECTION('axis',(0.,0.,1.));
#10251=DIRECTION('refdir',(1.,0.,0.));
#10252=DIRECTION('center_axis',(0.,0.,-1.));
#10253=DIRECTION('ref_axis',(1.,0.,0.));
#10254=DIRECTION('center_axis',(0.,0.,1.));
#10255=DIRECTION('ref_axis',(1.,0.,0.));
#10256=DIRECTION('center_axis',(0.,0.,-1.));
#10257=DIRECTION('ref_axis',(1.,0.,0.));
#10258=DIRECTION('center_axis',(0.,0.,1.));
#10259=DIRECTION('ref_axis',(1.,0.,0.));
#10260=DIRECTION('center_axis',(0.,0.,-1.));
#10261=DIRECTION('ref_axis',(1.,0.,0.));
#10262=DIRECTION('center_axis',(0.,0.,1.));
#10263=DIRECTION('ref_axis',(1.,0.,0.));
#10264=DIRECTION('center_axis',(0.,0.,-1.));
#10265=DIRECTION('ref_axis',(1.,0.,0.));
#10266=DIRECTION('center_axis',(0.,0.,1.));
#10267=DIRECTION('ref_axis',(1.,0.,0.));
#10268=DIRECTION('center_axis',(4.10828654779316E-33,-1.13946463231163E-19,
1.));
#10269=DIRECTION('ref_axis',(1.,0.,-4.10828654779316E-33));
#10270=DIRECTION('',(0.,1.,1.13946463231163E-19));
#10271=DIRECTION('',(0.,-1.,-1.13946463231163E-19));
#10272=DIRECTION('center_axis',(4.10828654779316E-33,-1.13946463231163E-19,
1.));
#10273=DIRECTION('ref_axis',(1.,0.,0.));
#10274=DIRECTION('center_axis',(4.10828654779316E-33,-1.13946463231163E-19,
1.));
#10275=DIRECTION('ref_axis',(1.,0.,0.));
#10276=DIRECTION('center_axis',(4.10828654779316E-33,-1.13946463231163E-19,
1.));
#10277=DIRECTION('ref_axis',(1.,0.,0.));
#10278=DIRECTION('center_axis',(0.,0.,-1.));
#10279=DIRECTION('ref_axis',(1.,0.,0.));
#10280=DIRECTION('center_axis',(-4.10828654779316E-33,1.13946463231163E-19,
-1.));
#10281=DIRECTION('ref_axis',(1.,0.,0.));
#10282=DIRECTION('',(0.,0.,-1.));
#10283=DIRECTION('center_axis',(0.,0.,-1.));
#10284=DIRECTION('ref_axis',(1.,0.,0.));
#10285=DIRECTION('center_axis',(-4.10828654779316E-33,1.13946463231163E-19,
-1.));
#10286=DIRECTION('ref_axis',(1.,0.,0.));
#10287=DIRECTION('',(0.,0.,-1.));
#10288=DIRECTION('center_axis',(4.10828654779316E-33,-1.13946463231163E-19,
1.));
#10289=DIRECTION('ref_axis',(1.,0.,0.));
#10290=DIRECTION('center_axis',(0.,0.,-1.));
#10291=DIRECTION('ref_axis',(1.,0.,0.));
#10292=DIRECTION('center_axis',(-4.10828654779316E-33,1.13946463231163E-19,
-1.));
#10293=DIRECTION('ref_axis',(1.,0.,0.));
#10294=DIRECTION('',(0.,0.,-1.));
#10295=DIRECTION('center_axis',(4.10828654779316E-33,-1.13946463231163E-19,
1.));
#10296=DIRECTION('ref_axis',(1.,0.,0.));
#10297=DIRECTION('center_axis',(0.,0.,-1.));
#10298=DIRECTION('ref_axis',(1.,0.,0.));
#10299=DIRECTION('center_axis',(-4.10828654779316E-33,1.13946463231163E-19,
-1.));
#10300=DIRECTION('ref_axis',(1.,0.,0.));
#10301=DIRECTION('',(0.,0.,-1.));
#10302=DIRECTION('center_axis',(0.,0.,-1.));
#10303=DIRECTION('ref_axis',(1.,0.,0.));
#10304=DIRECTION('center_axis',(-4.10828654779316E-33,1.13946463231163E-19,
-1.));
#10305=DIRECTION('ref_axis',(1.,0.,0.));
#10306=DIRECTION('',(0.,0.,-1.));
#10307=DIRECTION('center_axis',(0.,0.,-1.));
#10308=DIRECTION('ref_axis',(1.,0.,0.));
#10309=DIRECTION('center_axis',(0.,0.,-1.));
#10310=DIRECTION('ref_axis',(1.,0.,0.));
#10311=DIRECTION('center_axis',(0.,0.,1.));
#10312=DIRECTION('ref_axis',(1.,0.,0.));
#10313=DIRECTION('center_axis',(0.,0.,-1.));
#10314=DIRECTION('ref_axis',(1.,0.,0.));
#10315=DIRECTION('center_axis',(-4.10828654779316E-33,1.13946463231163E-19,
-1.));
#10316=DIRECTION('ref_axis',(1.,0.,0.));
#10317=DIRECTION('',(0.,0.,-1.));
#10318=DIRECTION('center_axis',(0.,0.,-1.));
#10319=DIRECTION('ref_axis',(1.,0.,0.));
#10320=DIRECTION('center_axis',(0.,0.,-1.));
#10321=DIRECTION('ref_axis',(1.,0.,0.));
#10322=DIRECTION('center_axis',(0.,0.,1.));
#10323=DIRECTION('ref_axis',(1.,0.,0.));
#10324=DIRECTION('center_axis',(0.,0.,-1.));
#10325=DIRECTION('ref_axis',(1.,0.,0.));
#10326=DIRECTION('',(0.,0.,-1.));
#10327=DIRECTION('center_axis',(0.,0.,1.));
#10328=DIRECTION('ref_axis',(1.,0.,0.));
#10329=DIRECTION('center_axis',(0.,0.,-1.));
#10330=DIRECTION('ref_axis',(1.,0.,0.));
#10331=DIRECTION('',(0.,0.,-1.));
#10332=DIRECTION('center_axis',(0.,0.,1.));
#10333=DIRECTION('ref_axis',(1.,0.,0.));
#10334=DIRECTION('center_axis',(0.,-1.,0.));
#10335=DIRECTION('ref_axis',(-1.,0.,0.));
#10336=DIRECTION('',(0.0523359562429438,0.,0.998629534754574));
#10337=DIRECTION('',(1.,0.,0.));
#10338=DIRECTION('',(-0.0523359562429438,0.,-0.998629534754574));
#10339=DIRECTION('',(1.,0.,0.));
#10340=DIRECTION('center_axis',(0.,-1.,0.));
#10341=DIRECTION('ref_axis',(-1.,0.,0.));
#10342=DIRECTION('',(0.,0.,-1.));
#10343=DIRECTION('',(1.,0.,0.));
#10344=DIRECTION('',(0.,0.,1.));
#10345=DIRECTION('',(1.,0.,0.));
#10346=DIRECTION('center_axis',(0.,-1.,0.));
#10347=DIRECTION('ref_axis',(-1.,0.,0.));
#10348=DIRECTION('',(0.,0.,-1.));
#10349=DIRECTION('',(1.,0.,0.));
#10350=DIRECTION('',(0.,0.,1.));
#10351=DIRECTION('',(1.,0.,0.));
#10352=DIRECTION('center_axis',(0.,-1.,0.));
#10353=DIRECTION('ref_axis',(-1.,0.,0.));
#10354=DIRECTION('',(0.,0.,-1.));
#10355=DIRECTION('',(1.,0.,0.));
#10356=DIRECTION('',(0.,0.,1.));
#10357=DIRECTION('',(1.,0.,0.));
#10358=DIRECTION('center_axis',(0.,1.,0.));
#10359=DIRECTION('ref_axis',(1.,0.,0.));
#10360=DIRECTION('',(-0.0523359562429438,0.,-0.998629534754574));
#10361=DIRECTION('',(-1.,0.,0.));
#10362=DIRECTION('',(0.0523359562429438,0.,0.998629534754574));
#10363=DIRECTION('',(-1.,0.,0.));
#10364=DIRECTION('center_axis',(0.,1.,0.));
#10365=DIRECTION('ref_axis',(1.,0.,0.));
#10366=DIRECTION('',(0.,0.,1.));
#10367=DIRECTION('',(-1.,0.,0.));
#10368=DIRECTION('',(0.,0.,-1.));
#10369=DIRECTION('',(-1.,0.,0.));
#10370=DIRECTION('center_axis',(0.,1.,0.));
#10371=DIRECTION('ref_axis',(1.,0.,0.));
#10372=DIRECTION('',(0.,0.,1.));
#10373=DIRECTION('',(-1.,0.,0.));
#10374=DIRECTION('',(0.,0.,-1.));
#10375=DIRECTION('',(-1.,0.,0.));
#10376=DIRECTION('center_axis',(0.,0.,1.));
#10377=DIRECTION('ref_axis',(1.,0.,0.));
#10378=DIRECTION('center_axis',(0.,0.,1.));
#10379=DIRECTION('ref_axis',(1.,0.,0.));
#10380=DIRECTION('center_axis',(0.,0.,1.));
#10381=DIRECTION('ref_axis',(1.,0.,0.));
#10382=DIRECTION('center_axis',(0.,0.,1.));
#10383=DIRECTION('ref_axis',(1.,0.,0.));
#10384=DIRECTION('center_axis',(0.,0.,1.));
#10385=DIRECTION('ref_axis',(1.,0.,0.));
#10386=DIRECTION('',(0.,1.,0.));
#10387=DIRECTION('',(0.,-1.,0.));
#10388=DIRECTION('center_axis',(0.,0.,1.));
#10389=DIRECTION('ref_axis',(1.,0.,0.));
#10390=DIRECTION('',(0.,-1.,0.));
#10391=DIRECTION('',(0.,1.,0.));
#10392=DIRECTION('center_axis',(0.,0.,1.));
#10393=DIRECTION('ref_axis',(1.,0.,0.));
#10394=DIRECTION('',(0.,-1.,0.));
#10395=DIRECTION('',(0.,1.,0.));
#10396=DIRECTION('center_axis',(0.,0.,1.));
#10397=DIRECTION('ref_axis',(1.,0.,0.));
#10398=DIRECTION('',(0.,-1.,0.));
#10399=DIRECTION('',(-1.,0.,0.));
#10400=DIRECTION('',(0.,1.,0.));
#10401=DIRECTION('center_axis',(0.,1.,0.));
#10402=DIRECTION('ref_axis',(1.,0.,0.));
#10403=DIRECTION('',(0.,0.,1.));
#10404=DIRECTION('',(-1.,0.,0.));
#10405=DIRECTION('',(0.,0.,-1.));
#10406=DIRECTION('center_axis',(-1.,0.,0.));
#10407=DIRECTION('ref_axis',(0.,-1.,0.));
#10408=DIRECTION('',(0.,-1.,0.));
#10409=DIRECTION('center_axis',(1.,0.,0.));
#10410=DIRECTION('ref_axis',(0.,1.,0.));
#10411=DIRECTION('',(0.,1.,0.));
#10412=DIRECTION('',(0.,1.,0.));
#10413=DIRECTION('center_axis',(1.,0.,0.));
#10414=DIRECTION('ref_axis',(0.,1.,0.));
#10415=DIRECTION('',(0.,1.,0.));
#10416=DIRECTION('',(0.,1.,1.13946463231163E-19));
#10417=DIRECTION('',(0.,1.,0.));
#10418=DIRECTION('center_axis',(1.,0.,0.));
#10419=DIRECTION('ref_axis',(0.,1.,0.));
#10420=DIRECTION('',(0.,1.,0.));
#10421=DIRECTION('',(0.,1.,1.13946463231163E-19));
#10422=DIRECTION('',(0.,1.,0.));
#10423=DIRECTION('center_axis',(0.998629534754574,0.,-0.0523359562429438));
#10424=DIRECTION('ref_axis',(-0.0523359562429438,0.,-0.998629534754574));
#10425=DIRECTION('',(0.,-1.,0.));
#10426=DIRECTION('',(-5.97168109510197E-21,-1.,-1.13946463231163E-19));
#10427=DIRECTION('',(0.,-1.,0.));
#10428=DIRECTION('center_axis',(0.,0.,1.));
#10429=DIRECTION('ref_axis',(1.,0.,0.));
#10430=DIRECTION('',(0.,-1.,0.));
#10431=DIRECTION('',(0.,-1.,0.));
#10432=DIRECTION('',(0.,-1.,0.));
#10433=DIRECTION('',(0.,1.,0.));
#10434=DIRECTION('',(0.,-1.,0.));
#10435=DIRECTION('',(0.,1.,0.));
#10436=DIRECTION('',(0.,-1.,0.));
#10437=DIRECTION('',(0.,-1.,0.));
#10438=DIRECTION('',(0.,-1.,0.));
#10439=DIRECTION('',(0.,1.,0.));
#10440=DIRECTION('',(0.,1.,0.));
#10441=DIRECTION('center_axis',(0.,0.,1.));
#10442=DIRECTION('ref_axis',(1.,0.,0.));
#10443=DIRECTION('',(0.,0.,-1.));
#10444=DIRECTION('center_axis',(0.,0.,1.));
#10445=DIRECTION('ref_axis',(1.,0.,0.));
#10446=DIRECTION('center_axis',(4.10828654779316E-33,-1.13946463231163E-19,
1.));
#10447=DIRECTION('ref_axis',(1.,0.,0.));
#10448=DIRECTION('',(0.,0.,-1.));
#10449=DIRECTION('center_axis',(1.,0.,0.));
#10450=DIRECTION('ref_axis',(0.,1.,0.));
#10451=DIRECTION('',(0.,1.,1.13946463231163E-19));
#10452=DIRECTION('center_axis',(0.99852593895705,0.0542765992849681,9.38276897523041E-9));
#10453=DIRECTION('ref_axis',(0.0541946171271057,-0.99701772369063,0.0549418066794405));
#10454=DIRECTION('center_axis',(4.10828654779316E-33,-1.13946463231163E-19,
1.));
#10455=DIRECTION('ref_axis',(1.,0.,-4.10828654779316E-33));
#10456=DIRECTION('',(5.97168109510217E-21,-1.,-1.13946463231163E-19));
#10457=DIRECTION('center_axis',(-1.,0.,0.));
#10458=DIRECTION('ref_axis',(0.,-1.,0.));
#10459=DIRECTION('',(0.,-1.,-1.13946463231163E-19));
#10460=DIRECTION('center_axis',(4.10828654779316E-33,-1.13946463231163E-19,
1.));
#10461=DIRECTION('ref_axis',(1.,0.,-4.10828654779316E-33));
#10462=DIRECTION('center_axis',(-1.,0.,0.));
#10463=DIRECTION('ref_axis',(0.,-1.,0.));
#10464=DIRECTION('',(0.,-1.,-1.13946463231163E-19));
#10465=DIRECTION('center_axis',(4.10828654779316E-33,-1.13946463231163E-19,
1.));
#10466=DIRECTION('ref_axis',(1.,0.,-4.10828654779316E-33));
#10467=DIRECTION('center_axis',(-1.,0.,0.));
#10468=DIRECTION('ref_axis',(0.,-1.,0.));
#10469=DIRECTION('',(0.,-1.,-1.13946463231163E-19));
#10470=DIRECTION('center_axis',(-0.996961060527779,0.0779015005717205,0.));
#10471=DIRECTION('ref_axis',(0.,0.,1.));
#10472=DIRECTION('center_axis',(4.10828654779316E-33,-1.13946463231163E-19,
1.));
#10473=DIRECTION('ref_axis',(1.,0.,-4.10828654779316E-33));
#10474=DIRECTION('',(5.97168109510197E-21,1.,1.13946463231163E-19));
#10475=DIRECTION('center_axis',(-0.996961060527779,-0.0779015005717276,
-4.485055189269E-15));
#10476=DIRECTION('ref_axis',(-0.0777791112471086,0.995394757055134,0.0560329142626144));
#10477=DIRECTION('center_axis',(-0.377317868652411,-0.840644185582845,0.388521015186253));
#10478=DIRECTION('ref_axis',(-0.58566693710526,0.541587807512093,0.603056287203763));
#10479=DIRECTION('center_axis',(7.41164423166535E-16,1.,0.));
#10480=DIRECTION('ref_axis',(0.,0.,1.));
#10481=DIRECTION('center_axis',(0.0522650005536027,-0.0520548592672972,
0.997275619547472));
#10482=DIRECTION('ref_axis',(-0.998629534754574,7.40148683083438E-16,0.0523359562429445));
#10483=DIRECTION('center_axis',(0.376559988603802,-0.837471124372148,0.396036224133039));
#10484=DIRECTION('ref_axis',(0.577069986161316,0.546481578685729,0.606916893181374));
#10485=DIRECTION('center_axis',(0.998525938475037,-0.0542766081525538,0.));
#10486=DIRECTION('ref_axis',(0.,0.,1.));
#10487=DIRECTION('center_axis',(-0.0522648366634829,-0.0521149007022807,
0.997272492337641));
#10488=DIRECTION('ref_axis',(0.0541946171271058,0.99701772369063,0.0549418066794413));
#10489=DIRECTION('center_axis',(5.32220538281047E-11,1.,-1.01553728389566E-9));
#10490=DIRECTION('ref_axis',(0.998629534754574,0.,0.0523359562429456));
#10491=DIRECTION('center_axis',(0.37731786865241,-0.840644185582843,-0.388521015186259));
#10492=DIRECTION('ref_axis',(-0.585666937105255,-0.541587807512095,0.603056287203766));
#10493=DIRECTION('center_axis',(0.0522650005536027,0.0520548592672965,0.997275619547472));
#10494=DIRECTION('ref_axis',(-0.0777791112471059,-0.995394757055134,0.0560329142626137));
#10495=DIRECTION('center_axis',(0.,-1.,0.));
#10496=DIRECTION('ref_axis',(-0.998629534754574,0.,0.0523359562429439));
#10497=DIRECTION('center_axis',(5.97168109510197E-21,1.,1.13946463231163E-19));
#10498=DIRECTION('ref_axis',(-0.688354575693753,0.,0.725374371012288));
#10499=DIRECTION('center_axis',(-0.376559987018669,-0.837471124206646,-0.396036225990193));
#10500=DIRECTION('ref_axis',(0.577069983350267,-0.54648157893936,0.606916895625808));
#10501=DIRECTION('center_axis',(-0.0522648366634817,0.0521149007022785,
0.997272492337641));
#10502=DIRECTION('ref_axis',(0.998629534754574,0.,0.052335956242946));
#10503=DIRECTION('center_axis',(1.01693095242295E-9,-1.,0.));
#10504=DIRECTION('ref_axis',(0.,0.,1.));
#10505=DIRECTION('center_axis',(5.97168109510217E-21,-1.,-1.13946463231163E-19));
#10506=DIRECTION('ref_axis',(0.688354575693753,0.,0.725374371012289));
#10507=DIRECTION('',(-5.97168109510217E-21,1.,1.13946463231163E-19));
#10508=DIRECTION('center_axis',(-0.998629534754574,0.,-0.0523359562429455));
#10509=DIRECTION('ref_axis',(-0.0523359562429455,0.,0.998629534754574));
#10510=DIRECTION('center_axis',(-0.377317868652411,-0.840644185582845,0.388521015186254));
#10511=DIRECTION('ref_axis',(-0.585666937105261,0.541587807512092,0.603056287203763));
#10512=DIRECTION('center_axis',(7.41164423166535E-16,1.,0.));
#10513=DIRECTION('ref_axis',(0.,0.,1.));
#10514=DIRECTION('center_axis',(-0.996961060527779,-0.0779015005717276,
-4.485055189269E-15));
#10515=DIRECTION('ref_axis',(-0.0777791112471086,0.995394757055134,0.0560329142626144));
#10516=DIRECTION('center_axis',(0.0522650005536027,-0.0520548592672972,
0.997275619547472));
#10517=DIRECTION('ref_axis',(-0.998629534754574,7.40148683083438E-16,0.0523359562429445));
#10518=DIRECTION('center_axis',(0.376559988603802,-0.837471124372148,0.396036224133039));
#10519=DIRECTION('ref_axis',(0.577069986161311,0.546481578685732,0.606916893181376));
#10520=DIRECTION('center_axis',(0.998525938475037,-0.0542766081525538,0.));
#10521=DIRECTION('ref_axis',(0.,0.,1.));
#10522=DIRECTION('center_axis',(5.32220538281047E-11,1.,-1.01553728389566E-9));
#10523=DIRECTION('ref_axis',(0.998629534754574,0.,0.0523359562429456));
#10524=DIRECTION('center_axis',(-0.0522648366634829,-0.0521149007022807,
0.997272492337641));
#10525=DIRECTION('ref_axis',(0.0541946171271058,0.99701772369063,0.0549418066794413));
#10526=DIRECTION('center_axis',(0.37731786865241,-0.840644185582843,-0.388521015186259));
#10527=DIRECTION('ref_axis',(-0.585666937105255,-0.541587807512095,0.603056287203766));
#10528=DIRECTION('center_axis',(-0.996961060527779,0.0779015005717205,0.));
#10529=DIRECTION('ref_axis',(0.,0.,1.));
#10530=DIRECTION('center_axis',(0.,-1.,0.));
#10531=DIRECTION('ref_axis',(-0.998629534754574,0.,0.0523359562429439));
#10532=DIRECTION('center_axis',(0.0522650005536027,0.0520548592672965,0.997275619547472));
#10533=DIRECTION('ref_axis',(-0.0777791112471059,-0.995394757055134,0.0560329142626137));
#10534=DIRECTION('center_axis',(5.97168109510197E-21,1.,1.13946463231163E-19));
#10535=DIRECTION('ref_axis',(-0.688354575693753,0.,0.725374371012289));
#10536=DIRECTION('',(-5.97168109510197E-21,-1.,-1.13946463231163E-19));
#10537=DIRECTION('',(5.97168109510197E-21,1.,1.13946463231163E-19));
#10538=DIRECTION('center_axis',(-0.376559987018669,-0.837471124206646,-0.396036225990194));
#10539=DIRECTION('ref_axis',(0.577069983350267,-0.546481578939359,0.606916895625808));
#10540=DIRECTION('center_axis',(-0.0522648366634817,0.0521149007022785,
0.997272492337641));
#10541=DIRECTION('ref_axis',(0.998629534754574,0.,0.052335956242946));
#10542=DIRECTION('center_axis',(1.01693095242295E-9,-1.,0.));
#10543=DIRECTION('ref_axis',(0.,0.,1.));
#10544=DIRECTION('center_axis',(0.99852593895705,0.0542765992849681,9.38276897523041E-9));
#10545=DIRECTION('ref_axis',(0.0541946171271057,-0.99701772369063,0.0549418066794405));
#10546=DIRECTION('center_axis',(5.97168109510217E-21,-1.,-1.13946463231163E-19));
#10547=DIRECTION('ref_axis',(0.688354575693753,0.,0.725374371012289));
#10548=DIRECTION('',(-5.97168109510217E-21,1.,1.13946463231163E-19));
#10549=DIRECTION('',(5.97168109510217E-21,-1.,-1.13946463231163E-19));
#10550=DIRECTION('center_axis',(0.998629534754574,0.,-0.0523359562429438));
#10551=DIRECTION('ref_axis',(-0.0523359562429438,0.,-0.998629534754574));
#10552=DIRECTION('center_axis',(4.10828654779316E-33,-1.13946463231163E-19,
1.));
#10553=DIRECTION('ref_axis',(1.,0.,-4.10828654779316E-33));
#10554=DIRECTION('center_axis',(-0.998629534754574,0.,-0.0523359562429455));
#10555=DIRECTION('ref_axis',(-0.0523359562429455,0.,0.998629534754574));
#10556=DIRECTION('axis',(0.,0.,1.));
#10557=DIRECTION('refdir',(1.,0.,0.));
#10558=DIRECTION('center_axis',(0.,0.,-1.));
#10559=DIRECTION('ref_axis',(1.,0.,0.));
#10560=DIRECTION('center_axis',(0.,0.,1.));
#10561=DIRECTION('ref_axis',(1.,0.,0.));
#10562=DIRECTION('center_axis',(0.,0.,-1.));
#10563=DIRECTION('ref_axis',(1.,0.,0.));
#10564=DIRECTION('center_axis',(0.,0.,1.));
#10565=DIRECTION('ref_axis',(1.,0.,0.));
#10566=DIRECTION('center_axis',(0.,0.,-1.));
#10567=DIRECTION('ref_axis',(1.,0.,0.));
#10568=DIRECTION('center_axis',(0.,0.,1.));
#10569=DIRECTION('ref_axis',(1.,0.,0.));
#10570=DIRECTION('center_axis',(0.,0.,-1.));
#10571=DIRECTION('ref_axis',(1.,0.,0.));
#10572=DIRECTION('center_axis',(0.,0.,1.));
#10573=DIRECTION('ref_axis',(1.,0.,0.));
#10574=DIRECTION('center_axis',(4.10828654779316E-33,-1.13946463231163E-19,
1.));
#10575=DIRECTION('ref_axis',(1.,0.,-4.10828654779316E-33));
#10576=DIRECTION('',(0.,1.,1.13946463231163E-19));
#10577=DIRECTION('',(0.,-1.,-1.13946463231163E-19));
#10578=DIRECTION('center_axis',(4.10828654779316E-33,-1.13946463231163E-19,
1.));
#10579=DIRECTION('ref_axis',(1.,0.,0.));
#10580=DIRECTION('center_axis',(4.10828654779316E-33,-1.13946463231163E-19,
1.));
#10581=DIRECTION('ref_axis',(1.,0.,0.));
#10582=DIRECTION('center_axis',(4.10828654779316E-33,-1.13946463231163E-19,
1.));
#10583=DIRECTION('ref_axis',(1.,0.,0.));
#10584=DIRECTION('center_axis',(0.86602540378444,0.499999999999998,0.));
#10585=DIRECTION('ref_axis',(0.499999999999998,-0.86602540378444,0.));
#10586=DIRECTION('',(0.499999999999998,-0.86602540378444,-9.86805318295791E-20));
#10587=DIRECTION('',(0.,0.,-1.));
#10588=DIRECTION('',(0.499999999999998,-0.86602540378444,0.));
#10589=DIRECTION('',(0.,0.,-1.));
#10590=DIRECTION('center_axis',(1.60246890531964E-16,1.,0.));
#10591=DIRECTION('ref_axis',(1.,-1.60246890531964E-16,0.));
#10592=DIRECTION('',(1.,-1.60246890531964E-16,-4.12654611421307E-33));
#10593=DIRECTION('',(0.,0.,-1.));
#10594=DIRECTION('',(1.,-1.60246890531964E-16,0.));
#10595=DIRECTION('center_axis',(-0.86602540378444,0.499999999999998,0.));
#10596=DIRECTION('ref_axis',(0.499999999999998,0.86602540378444,0.));
#10597=DIRECTION('',(0.499999999999998,0.86602540378444,9.86805318295749E-20));
#10598=DIRECTION('',(0.,0.,-1.));
#10599=DIRECTION('',(0.499999999999998,0.86602540378444,0.));
#10600=DIRECTION('center_axis',(-0.86602540378444,-0.499999999999998,0.));
#10601=DIRECTION('ref_axis',(-0.499999999999998,0.86602540378444,0.));
#10602=DIRECTION('',(-0.499999999999998,0.86602540378444,9.86805318295791E-20));
#10603=DIRECTION('',(0.,0.,-1.));
#10604=DIRECTION('',(-0.499999999999998,0.86602540378444,0.));
#10605=DIRECTION('center_axis',(-1.60246890531964E-16,-1.,0.));
#10606=DIRECTION('ref_axis',(-1.,1.60246890531964E-16,0.));
#10607=DIRECTION('',(-1.,1.60246890531964E-16,4.12654611421307E-33));
#10608=DIRECTION('',(0.,0.,-1.));
#10609=DIRECTION('',(-1.,1.60246890531964E-16,0.));
#10610=DIRECTION('center_axis',(0.86602540378444,-0.499999999999998,0.));
#10611=DIRECTION('ref_axis',(-0.499999999999998,-0.86602540378444,0.));
#10612=DIRECTION('',(-0.499999999999998,-0.86602540378444,-9.86805318295749E-20));
#10613=DIRECTION('',(-0.499999999999998,-0.86602540378444,0.));
#10614=DIRECTION('center_axis',(0.,0.,-1.));
#10615=DIRECTION('ref_axis',(-1.,0.,0.));
#10616=DIRECTION('center_axis',(0.,0.,1.));
#10617=DIRECTION('ref_axis',(1.,0.,0.));
#10618=DIRECTION('center_axis',(0.866025403784439,0.5,0.));
#10619=DIRECTION('ref_axis',(0.5,-0.866025403784439,0.));
#10620=DIRECTION('',(0.5,-0.866025403784439,-9.86805318295789E-20));
#10621=DIRECTION('',(0.,0.,-1.));
#10622=DIRECTION('',(0.5,-0.866025403784439,0.));
#10623=DIRECTION('',(0.,0.,-1.));
#10624=DIRECTION('center_axis',(1.60246890531964E-16,1.,0.));
#10625=DIRECTION('ref_axis',(1.,-1.60246890531964E-16,0.));
#10626=DIRECTION('',(1.,-1.60246890531964E-16,-4.12654611421307E-33));
#10627=DIRECTION('',(0.,0.,-1.));
#10628=DIRECTION('',(1.,-1.60246890531964E-16,0.));
#10629=DIRECTION('center_axis',(-0.866025403784438,0.5,0.));
#10630=DIRECTION('ref_axis',(0.5,0.866025403784438,0.));
#10631=DIRECTION('',(0.5,0.866025403784438,9.86805318295748E-20));
#10632=DIRECTION('',(0.,0.,-1.));
#10633=DIRECTION('',(0.5,0.866025403784438,0.));
#10634=DIRECTION('center_axis',(-0.866025403784439,-0.499999999999999,0.));
#10635=DIRECTION('ref_axis',(-0.499999999999999,0.866025403784439,0.));
#10636=DIRECTION('',(-0.499999999999999,0.866025403784439,9.8680531829579E-20));
#10637=DIRECTION('',(0.,0.,-1.));
#10638=DIRECTION('',(-0.499999999999999,0.866025403784439,0.));
#10639=DIRECTION('center_axis',(-1.60246890531964E-16,-1.,0.));
#10640=DIRECTION('ref_axis',(-1.,1.60246890531964E-16,0.));
#10641=DIRECTION('',(-1.,1.60246890531964E-16,4.12654611421307E-33));
#10642=DIRECTION('',(0.,0.,-1.));
#10643=DIRECTION('',(-1.,1.60246890531964E-16,0.));
#10644=DIRECTION('center_axis',(0.866025403784439,-0.5,0.));
#10645=DIRECTION('ref_axis',(-0.5,-0.866025403784439,0.));
#10646=DIRECTION('',(-0.5,-0.866025403784439,-9.86805318295748E-20));
#10647=DIRECTION('',(-0.5,-0.866025403784439,0.));
#10648=DIRECTION('center_axis',(0.,0.,-1.));
#10649=DIRECTION('ref_axis',(-1.,0.,0.));
#10650=DIRECTION('center_axis',(0.,0.,1.));
#10651=DIRECTION('ref_axis',(1.,0.,0.));
#10652=DIRECTION('center_axis',(0.,0.,-1.));
#10653=DIRECTION('ref_axis',(1.,0.,0.));
#10654=DIRECTION('center_axis',(-4.10828654779316E-33,1.13946463231163E-19,
-1.));
#10655=DIRECTION('ref_axis',(1.,0.,0.));
#10656=DIRECTION('',(0.,0.,-1.));
#10657=DIRECTION('center_axis',(0.,0.,-1.));
#10658=DIRECTION('ref_axis',(1.,0.,0.));
#10659=DIRECTION('center_axis',(-4.10828654779316E-33,1.13946463231163E-19,
-1.));
#10660=DIRECTION('ref_axis',(1.,0.,0.));
#10661=DIRECTION('',(0.,0.,-1.));
#10662=DIRECTION('center_axis',(4.10828654779316E-33,-1.13946463231163E-19,
1.));
#10663=DIRECTION('ref_axis',(1.,0.,0.));
#10664=DIRECTION('center_axis',(0.,0.,-1.));
#10665=DIRECTION('ref_axis',(1.,0.,0.));
#10666=DIRECTION('center_axis',(-4.10828654779316E-33,1.13946463231163E-19,
-1.));
#10667=DIRECTION('ref_axis',(1.,0.,0.));
#10668=DIRECTION('',(0.,0.,-1.));
#10669=DIRECTION('center_axis',(4.10828654779316E-33,-1.13946463231163E-19,
1.));
#10670=DIRECTION('ref_axis',(1.,0.,0.));
#10671=DIRECTION('center_axis',(0.,0.,-1.));
#10672=DIRECTION('ref_axis',(1.,0.,0.));
#10673=DIRECTION('center_axis',(-4.10828654779316E-33,1.13946463231163E-19,
-1.));
#10674=DIRECTION('ref_axis',(1.,0.,0.));
#10675=DIRECTION('',(0.,0.,-1.));
#10676=DIRECTION('center_axis',(0.,0.,-1.));
#10677=DIRECTION('ref_axis',(1.,0.,0.));
#10678=DIRECTION('',(0.,0.,-1.));
#10679=DIRECTION('center_axis',(0.,0.,1.));
#10680=DIRECTION('ref_axis',(1.,0.,0.));
#10681=DIRECTION('center_axis',(0.,0.,-1.));
#10682=DIRECTION('ref_axis',(1.,0.,0.));
#10683=DIRECTION('',(0.,0.,-1.));
#10684=DIRECTION('center_axis',(0.,0.,1.));
#10685=DIRECTION('ref_axis',(1.,0.,0.));
#10686=DIRECTION('center_axis',(0.,-1.,0.));
#10687=DIRECTION('ref_axis',(-1.,0.,0.));
#10688=DIRECTION('',(0.0523359562429438,0.,0.998629534754574));
#10689=DIRECTION('',(1.,0.,0.));
#10690=DIRECTION('',(-0.0523359562429438,0.,-0.998629534754574));
#10691=DIRECTION('',(1.,0.,0.));
#10692=DIRECTION('center_axis',(0.,-1.,0.));
#10693=DIRECTION('ref_axis',(-1.,0.,0.));
#10694=DIRECTION('',(0.,0.,-1.));
#10695=DIRECTION('',(1.,0.,0.));
#10696=DIRECTION('',(0.,0.,1.));
#10697=DIRECTION('',(1.,0.,0.));
#10698=DIRECTION('center_axis',(0.,-1.,0.));
#10699=DIRECTION('ref_axis',(-1.,0.,0.));
#10700=DIRECTION('',(0.,0.,-1.));
#10701=DIRECTION('',(1.,0.,0.));
#10702=DIRECTION('',(0.,0.,1.));
#10703=DIRECTION('',(1.,0.,0.));
#10704=DIRECTION('center_axis',(0.,-1.,0.));
#10705=DIRECTION('ref_axis',(-1.,0.,0.));
#10706=DIRECTION('',(0.,0.,-1.));
#10707=DIRECTION('',(1.,0.,0.));
#10708=DIRECTION('',(0.,0.,1.));
#10709=DIRECTION('',(1.,0.,0.));
#10710=DIRECTION('center_axis',(0.,1.,0.));
#10711=DIRECTION('ref_axis',(1.,0.,0.));
#10712=DIRECTION('',(-0.0523359562429438,0.,-0.998629534754574));
#10713=DIRECTION('',(-1.,0.,0.));
#10714=DIRECTION('',(0.0523359562429438,0.,0.998629534754574));
#10715=DIRECTION('',(-1.,0.,0.));
#10716=DIRECTION('center_axis',(0.,1.,0.));
#10717=DIRECTION('ref_axis',(1.,0.,0.));
#10718=DIRECTION('',(0.,0.,1.));
#10719=DIRECTION('',(-1.,0.,0.));
#10720=DIRECTION('',(0.,0.,-1.));
#10721=DIRECTION('',(-1.,0.,0.));
#10722=DIRECTION('center_axis',(0.,1.,0.));
#10723=DIRECTION('ref_axis',(1.,0.,0.));
#10724=DIRECTION('',(0.,0.,1.));
#10725=DIRECTION('',(-1.,0.,0.));
#10726=DIRECTION('',(0.,0.,-1.));
#10727=DIRECTION('',(-1.,0.,0.));
#10728=DIRECTION('center_axis',(0.,0.,1.));
#10729=DIRECTION('ref_axis',(1.,0.,0.));
#10730=DIRECTION('center_axis',(0.,0.,1.));
#10731=DIRECTION('ref_axis',(1.,0.,0.));
#10732=DIRECTION('center_axis',(0.,0.,1.));
#10733=DIRECTION('ref_axis',(1.,0.,0.));
#10734=DIRECTION('center_axis',(0.,0.,1.));
#10735=DIRECTION('ref_axis',(1.,0.,0.));
#10736=DIRECTION('center_axis',(0.,0.,1.));
#10737=DIRECTION('ref_axis',(1.,0.,0.));
#10738=DIRECTION('',(0.,1.,0.));
#10739=DIRECTION('',(0.,-1.,0.));
#10740=DIRECTION('center_axis',(0.,0.,1.));
#10741=DIRECTION('ref_axis',(1.,0.,0.));
#10742=DIRECTION('',(0.,-1.,0.));
#10743=DIRECTION('',(0.,1.,0.));
#10744=DIRECTION('center_axis',(0.,0.,1.));
#10745=DIRECTION('ref_axis',(1.,0.,0.));
#10746=DIRECTION('',(0.,-1.,0.));
#10747=DIRECTION('',(0.,1.,0.));
#10748=DIRECTION('center_axis',(0.,0.,1.));
#10749=DIRECTION('ref_axis',(1.,0.,0.));
#10750=DIRECTION('',(0.,-1.,0.));
#10751=DIRECTION('',(-1.,0.,0.));
#10752=DIRECTION('',(0.,1.,0.));
#10753=DIRECTION('center_axis',(0.,1.,0.));
#10754=DIRECTION('ref_axis',(1.,0.,0.));
#10755=DIRECTION('',(0.,0.,1.));
#10756=DIRECTION('',(-1.,0.,0.));
#10757=DIRECTION('',(0.,0.,-1.));
#10758=DIRECTION('center_axis',(-1.,0.,0.));
#10759=DIRECTION('ref_axis',(0.,-1.,0.));
#10760=DIRECTION('',(0.,-1.,0.));
#10761=DIRECTION('center_axis',(1.,0.,0.));
#10762=DIRECTION('ref_axis',(0.,1.,0.));
#10763=DIRECTION('',(0.,1.,0.));
#10764=DIRECTION('',(0.,1.,0.));
#10765=DIRECTION('center_axis',(1.,0.,0.));
#10766=DIRECTION('ref_axis',(0.,1.,0.));
#10767=DIRECTION('',(0.,1.,0.));
#10768=DIRECTION('',(0.,1.,1.13946463231163E-19));
#10769=DIRECTION('',(0.,1.,0.));
#10770=DIRECTION('center_axis',(1.,0.,0.));
#10771=DIRECTION('ref_axis',(0.,1.,0.));
#10772=DIRECTION('',(0.,1.,0.));
#10773=DIRECTION('',(0.,1.,1.13946463231163E-19));
#10774=DIRECTION('',(0.,1.,0.));
#10775=DIRECTION('center_axis',(0.998629534754574,0.,-0.0523359562429438));
#10776=DIRECTION('ref_axis',(-0.0523359562429438,0.,-0.998629534754574));
#10777=DIRECTION('',(0.,-1.,0.));
#10778=DIRECTION('',(-5.97168109510197E-21,-1.,-1.13946463231163E-19));
#10779=DIRECTION('',(0.,-1.,0.));
#10780=DIRECTION('center_axis',(0.,0.,1.));
#10781=DIRECTION('ref_axis',(1.,0.,0.));
#10782=DIRECTION('',(0.,-1.,0.));
#10783=DIRECTION('',(0.,-1.,0.));
#10784=DIRECTION('',(0.,-1.,0.));
#10785=DIRECTION('',(0.,1.,0.));
#10786=DIRECTION('',(0.,-1.,0.));
#10787=DIRECTION('',(0.,1.,0.));
#10788=DIRECTION('',(0.,-1.,0.));
#10789=DIRECTION('',(0.,-1.,0.));
#10790=DIRECTION('',(0.,-1.,0.));
#10791=DIRECTION('',(0.,1.,0.));
#10792=DIRECTION('',(0.,1.,0.));
#10793=DIRECTION('center_axis',(0.,0.,1.));
#10794=DIRECTION('ref_axis',(1.,0.,0.));
#10795=DIRECTION('',(0.,0.,-1.));
#10796=DIRECTION('center_axis',(0.,0.,1.));
#10797=DIRECTION('ref_axis',(1.,0.,0.));
#10798=DIRECTION('center_axis',(4.10828654779316E-33,-1.13946463231163E-19,
1.));
#10799=DIRECTION('ref_axis',(1.,0.,0.));
#10800=DIRECTION('',(0.,0.,-1.));
#10801=DIRECTION('center_axis',(1.,0.,0.));
#10802=DIRECTION('ref_axis',(0.,1.,0.));
#10803=DIRECTION('',(0.,1.,1.13946463231163E-19));
#10804=DIRECTION('center_axis',(0.99852593895705,0.0542765992849681,9.38276897523041E-9));
#10805=DIRECTION('ref_axis',(0.0541946171271057,-0.99701772369063,0.0549418066794405));
#10806=DIRECTION('center_axis',(4.10828654779316E-33,-1.13946463231163E-19,
1.));
#10807=DIRECTION('ref_axis',(1.,0.,-4.10828654779316E-33));
#10808=DIRECTION('',(5.97168109510217E-21,-1.,-1.13946463231163E-19));
#10809=DIRECTION('center_axis',(-1.,0.,0.));
#10810=DIRECTION('ref_axis',(0.,-1.,0.));
#10811=DIRECTION('',(0.,-1.,-1.13946463231163E-19));
#10812=DIRECTION('center_axis',(4.10828654779316E-33,-1.13946463231163E-19,
1.));
#10813=DIRECTION('ref_axis',(1.,0.,-4.10828654779316E-33));
#10814=DIRECTION('center_axis',(-1.,0.,0.));
#10815=DIRECTION('ref_axis',(0.,-1.,0.));
#10816=DIRECTION('',(0.,-1.,-1.13946463231163E-19));
#10817=DIRECTION('center_axis',(4.10828654779316E-33,-1.13946463231163E-19,
1.));
#10818=DIRECTION('ref_axis',(1.,0.,-4.10828654779316E-33));
#10819=DIRECTION('center_axis',(-1.,0.,0.));
#10820=DIRECTION('ref_axis',(0.,-1.,0.));
#10821=DIRECTION('',(0.,-1.,-1.13946463231163E-19));
#10822=DIRECTION('center_axis',(-0.996961060527779,0.0779015005717205,0.));
#10823=DIRECTION('ref_axis',(0.,0.,1.));
#10824=DIRECTION('center_axis',(4.10828654779316E-33,-1.13946463231163E-19,
1.));
#10825=DIRECTION('ref_axis',(1.,0.,-4.10828654779316E-33));
#10826=DIRECTION('',(5.97168109510197E-21,1.,1.13946463231163E-19));
#10827=DIRECTION('center_axis',(-0.996961060527779,-0.0779015005717276,
-4.485055189269E-15));
#10828=DIRECTION('ref_axis',(-0.0777791112471086,0.995394757055134,0.0560329142626144));
#10829=DIRECTION('center_axis',(-0.377317868652411,-0.840644185582845,0.388521015186253));
#10830=DIRECTION('ref_axis',(-0.58566693710526,0.541587807512093,0.603056287203763));
#10831=DIRECTION('center_axis',(7.41164423166535E-16,1.,0.));
#10832=DIRECTION('ref_axis',(0.,0.,1.));
#10833=DIRECTION('center_axis',(0.0522650005536027,-0.0520548592672972,
0.997275619547472));
#10834=DIRECTION('ref_axis',(-0.998629534754574,7.40148683083438E-16,0.0523359562429445));
#10835=DIRECTION('center_axis',(0.376559988603802,-0.837471124372148,0.396036224133039));
#10836=DIRECTION('ref_axis',(0.577069986161316,0.546481578685729,0.606916893181374));
#10837=DIRECTION('center_axis',(0.998525938475037,-0.0542766081525538,0.));
#10838=DIRECTION('ref_axis',(0.,0.,1.));
#10839=DIRECTION('center_axis',(-0.0522648366634829,-0.0521149007022807,
0.997272492337641));
#10840=DIRECTION('ref_axis',(0.0541946171271058,0.99701772369063,0.0549418066794413));
#10841=DIRECTION('center_axis',(5.32220538281047E-11,1.,-1.01553728389566E-9));
#10842=DIRECTION('ref_axis',(0.998629534754574,0.,0.0523359562429456));
#10843=DIRECTION('center_axis',(0.37731786865241,-0.840644185582843,-0.388521015186259));
#10844=DIRECTION('ref_axis',(-0.585666937105255,-0.541587807512095,0.603056287203766));
#10845=DIRECTION('center_axis',(0.0522650005536027,0.0520548592672965,0.997275619547472));
#10846=DIRECTION('ref_axis',(-0.0777791112471059,-0.995394757055134,0.0560329142626137));
#10847=DIRECTION('center_axis',(0.,-1.,0.));
#10848=DIRECTION('ref_axis',(-0.998629534754574,0.,0.0523359562429439));
#10849=DIRECTION('center_axis',(5.97168109510197E-21,1.,1.13946463231163E-19));
#10850=DIRECTION('ref_axis',(-0.688354575693753,0.,0.725374371012288));
#10851=DIRECTION('center_axis',(-0.376559987018669,-0.837471124206646,-0.396036225990193));
#10852=DIRECTION('ref_axis',(0.577069983350267,-0.54648157893936,0.606916895625808));
#10853=DIRECTION('center_axis',(-0.0522648366634817,0.0521149007022785,
0.997272492337641));
#10854=DIRECTION('ref_axis',(0.998629534754574,0.,0.052335956242946));
#10855=DIRECTION('center_axis',(1.01693095242295E-9,-1.,0.));
#10856=DIRECTION('ref_axis',(0.,0.,1.));
#10857=DIRECTION('center_axis',(5.97168109510217E-21,-1.,-1.13946463231163E-19));
#10858=DIRECTION('ref_axis',(0.688354575693753,0.,0.725374371012289));
#10859=DIRECTION('',(-5.97168109510217E-21,1.,1.13946463231163E-19));
#10860=DIRECTION('center_axis',(-0.998629534754574,0.,-0.0523359562429455));
#10861=DIRECTION('ref_axis',(-0.0523359562429455,0.,0.998629534754574));
#10862=DIRECTION('center_axis',(-0.377317868652411,-0.840644185582845,0.388521015186254));
#10863=DIRECTION('ref_axis',(-0.585666937105261,0.541587807512092,0.603056287203763));
#10864=DIRECTION('center_axis',(7.41164423166535E-16,1.,0.));
#10865=DIRECTION('ref_axis',(0.,0.,1.));
#10866=DIRECTION('center_axis',(-0.996961060527779,-0.0779015005717276,
-4.485055189269E-15));
#10867=DIRECTION('ref_axis',(-0.0777791112471086,0.995394757055134,0.0560329142626144));
#10868=DIRECTION('center_axis',(0.0522650005536027,-0.0520548592672972,
0.997275619547472));
#10869=DIRECTION('ref_axis',(-0.998629534754574,7.40148683083438E-16,0.0523359562429445));
#10870=DIRECTION('center_axis',(0.376559988603802,-0.837471124372148,0.396036224133039));
#10871=DIRECTION('ref_axis',(0.577069986161311,0.546481578685732,0.606916893181376));
#10872=DIRECTION('center_axis',(0.998525938475037,-0.0542766081525538,0.));
#10873=DIRECTION('ref_axis',(0.,0.,1.));
#10874=DIRECTION('center_axis',(5.32220538281047E-11,1.,-1.01553728389566E-9));
#10875=DIRECTION('ref_axis',(0.998629534754574,0.,0.0523359562429456));
#10876=DIRECTION('center_axis',(-0.0522648366634829,-0.0521149007022807,
0.997272492337641));
#10877=DIRECTION('ref_axis',(0.0541946171271058,0.99701772369063,0.0549418066794413));
#10878=DIRECTION('center_axis',(0.37731786865241,-0.840644185582843,-0.388521015186259));
#10879=DIRECTION('ref_axis',(-0.585666937105255,-0.541587807512095,0.603056287203766));
#10880=DIRECTION('center_axis',(-0.996961060527779,0.0779015005717205,0.));
#10881=DIRECTION('ref_axis',(0.,0.,1.));
#10882=DIRECTION('center_axis',(0.,-1.,0.));
#10883=DIRECTION('ref_axis',(-0.998629534754574,0.,0.0523359562429439));
#10884=DIRECTION('center_axis',(0.0522650005536027,0.0520548592672965,0.997275619547472));
#10885=DIRECTION('ref_axis',(-0.0777791112471059,-0.995394757055134,0.0560329142626137));
#10886=DIRECTION('center_axis',(5.97168109510197E-21,1.,1.13946463231163E-19));
#10887=DIRECTION('ref_axis',(-0.688354575693753,0.,0.725374371012289));
#10888=DIRECTION('',(-5.97168109510197E-21,-1.,-1.13946463231163E-19));
#10889=DIRECTION('',(5.97168109510197E-21,1.,1.13946463231163E-19));
#10890=DIRECTION('center_axis',(-0.376559987018669,-0.837471124206646,-0.396036225990194));
#10891=DIRECTION('ref_axis',(0.577069983350267,-0.546481578939359,0.606916895625808));
#10892=DIRECTION('center_axis',(-0.0522648366634817,0.0521149007022785,
0.997272492337641));
#10893=DIRECTION('ref_axis',(0.998629534754574,0.,0.052335956242946));
#10894=DIRECTION('center_axis',(1.01693095242295E-9,-1.,0.));
#10895=DIRECTION('ref_axis',(0.,0.,1.));
#10896=DIRECTION('center_axis',(0.99852593895705,0.0542765992849681,9.38276897523041E-9));
#10897=DIRECTION('ref_axis',(0.0541946171271057,-0.99701772369063,0.0549418066794405));
#10898=DIRECTION('center_axis',(5.97168109510217E-21,-1.,-1.13946463231163E-19));
#10899=DIRECTION('ref_axis',(0.688354575693753,0.,0.725374371012289));
#10900=DIRECTION('',(-5.97168109510217E-21,1.,1.13946463231163E-19));
#10901=DIRECTION('',(5.97168109510217E-21,-1.,-1.13946463231163E-19));
#10902=DIRECTION('center_axis',(0.998629534754574,0.,-0.0523359562429438));
#10903=DIRECTION('ref_axis',(-0.0523359562429438,0.,-0.998629534754574));
#10904=DIRECTION('center_axis',(4.10828654779316E-33,-1.13946463231163E-19,
1.));
#10905=DIRECTION('ref_axis',(1.,0.,-4.10828654779316E-33));
#10906=DIRECTION('center_axis',(-0.998629534754574,0.,-0.0523359562429455));
#10907=DIRECTION('ref_axis',(-0.0523359562429455,0.,0.998629534754574));
#10908=DIRECTION('axis',(0.,0.,1.));
#10909=DIRECTION('refdir',(1.,0.,0.));
#10910=DIRECTION('center_axis',(0.,0.,1.));
#10911=DIRECTION('ref_axis',(1.,0.,0.));
#10912=DIRECTION('',(0.,0.,-1.));
#10913=DIRECTION('center_axis',(0.,0.,-1.));
#10914=DIRECTION('ref_axis',(1.,0.,0.));
#10915=DIRECTION('center_axis',(0.,0.,1.));
#10916=DIRECTION('ref_axis',(1.,0.,0.));
#10917=DIRECTION('',(0.,0.,-1.));
#10918=DIRECTION('center_axis',(0.,0.,1.));
#10919=DIRECTION('ref_axis',(1.,0.,0.));
#10920=DIRECTION('',(0.,0.,-1.));
#10921=DIRECTION('center_axis',(0.,0.,1.));
#10922=DIRECTION('ref_axis',(1.,0.,0.));
#10923=DIRECTION('',(0.,0.,-1.));
#10924=DIRECTION('center_axis',(0.,0.,1.));
#10925=DIRECTION('ref_axis',(1.,0.,0.));
#10926=DIRECTION('',(0.,0.,-1.));
#10927=DIRECTION('center_axis',(0.,0.,1.));
#10928=DIRECTION('ref_axis',(1.,0.,0.));
#10929=DIRECTION('',(0.,0.,-1.));
#10930=DIRECTION('center_axis',(0.,0.,1.));
#10931=DIRECTION('ref_axis',(1.,0.,0.));
#10932=DIRECTION('',(0.,0.,-1.));
#10933=DIRECTION('center_axis',(0.,0.,1.));
#10934=DIRECTION('ref_axis',(1.,0.,0.));
#10935=DIRECTION('',(0.,0.,-1.));
#10936=DIRECTION('center_axis',(0.,0.,1.));
#10937=DIRECTION('ref_axis',(1.,0.,0.));
#10938=DIRECTION('',(0.,0.,-1.));
#10939=DIRECTION('center_axis',(0.,0.,1.));
#10940=DIRECTION('ref_axis',(1.,0.,0.));
#10941=DIRECTION('',(0.,0.,-1.));
#10942=DIRECTION('center_axis',(0.,0.,1.));
#10943=DIRECTION('ref_axis',(1.,0.,0.));
#10944=DIRECTION('',(0.,0.,-1.));
#10945=DIRECTION('center_axis',(0.,0.,1.));
#10946=DIRECTION('ref_axis',(1.,0.,0.));
#10947=DIRECTION('',(0.,0.,-1.));
#10948=DIRECTION('center_axis',(0.,0.,1.));
#10949=DIRECTION('ref_axis',(1.,0.,0.));
#10950=DIRECTION('',(0.,0.,-1.));
#10951=DIRECTION('center_axis',(0.,0.,1.));
#10952=DIRECTION('ref_axis',(1.,0.,0.));
#10953=DIRECTION('',(0.,0.,-1.));
#10954=DIRECTION('center_axis',(0.,0.,1.));
#10955=DIRECTION('ref_axis',(1.,0.,0.));
#10956=DIRECTION('',(0.,0.,-1.));
#10957=DIRECTION('center_axis',(0.,0.,1.));
#10958=DIRECTION('ref_axis',(1.,0.,0.));
#10959=DIRECTION('',(0.,0.,-1.));
#10960=DIRECTION('center_axis',(0.,0.,1.));
#10961=DIRECTION('ref_axis',(1.,0.,0.));
#10962=DIRECTION('',(0.,0.,-1.));
#10963=DIRECTION('center_axis',(0.,0.,1.));
#10964=DIRECTION('ref_axis',(1.,0.,0.));
#10965=DIRECTION('',(0.,0.,-1.));
#10966=DIRECTION('center_axis',(0.,0.,1.));
#10967=DIRECTION('ref_axis',(1.,0.,0.));
#10968=DIRECTION('',(0.,0.,-1.));
#10969=DIRECTION('center_axis',(0.,0.,1.));
#10970=DIRECTION('ref_axis',(1.,0.,0.));
#10971=DIRECTION('',(0.,0.,-1.));
#10972=DIRECTION('center_axis',(0.,0.,1.));
#10973=DIRECTION('ref_axis',(1.,0.,0.));
#10974=DIRECTION('',(0.,0.,-1.));
#10975=DIRECTION('center_axis',(0.,0.,1.));
#10976=DIRECTION('ref_axis',(1.,0.,0.));
#10977=DIRECTION('',(0.,0.,-1.));
#10978=DIRECTION('center_axis',(0.,0.,1.));
#10979=DIRECTION('ref_axis',(1.,0.,0.));
#10980=DIRECTION('',(0.,0.,-1.));
#10981=DIRECTION('center_axis',(0.,0.,1.));
#10982=DIRECTION('ref_axis',(1.,0.,0.));
#10983=DIRECTION('',(0.,0.,-1.));
#10984=DIRECTION('center_axis',(0.,0.,1.));
#10985=DIRECTION('ref_axis',(1.,0.,0.));
#10986=DIRECTION('',(0.,0.,-1.));
#10987=DIRECTION('center_axis',(0.,0.,1.));
#10988=DIRECTION('ref_axis',(1.,0.,0.));
#10989=DIRECTION('',(0.,0.,-1.));
#10990=DIRECTION('center_axis',(0.,0.,1.));
#10991=DIRECTION('ref_axis',(1.,0.,0.));
#10992=DIRECTION('',(0.,0.,-1.));
#10993=DIRECTION('center_axis',(0.,0.,1.));
#10994=DIRECTION('ref_axis',(1.,0.,0.));
#10995=DIRECTION('',(0.,0.,-1.));
#10996=DIRECTION('center_axis',(0.,0.,1.));
#10997=DIRECTION('ref_axis',(1.,0.,0.));
#10998=DIRECTION('',(0.,0.,-1.));
#10999=DIRECTION('center_axis',(0.,0.,1.));
#11000=DIRECTION('ref_axis',(1.,0.,0.));
#11001=DIRECTION('',(0.,0.,-1.));
#11002=DIRECTION('center_axis',(0.,0.,1.));
#11003=DIRECTION('ref_axis',(1.,-2.42503376499884E-13,0.));
#11004=DIRECTION('',(0.,0.,1.));
#11005=DIRECTION('center_axis',(0.,0.,-1.));
#11006=DIRECTION('ref_axis',(1.,-2.42503376499884E-13,0.));
#11007=DIRECTION('center_axis',(0.,0.,1.));
#11008=DIRECTION('ref_axis',(1.,-2.42503376499884E-13,0.));
#11009=DIRECTION('',(0.,0.,1.));
#11010=DIRECTION('center_axis',(0.,0.,1.));
#11011=DIRECTION('ref_axis',(1.,-2.42503376499884E-13,0.));
#11012=DIRECTION('',(0.,0.,1.));
#11013=DIRECTION('center_axis',(0.,0.,1.));
#11014=DIRECTION('ref_axis',(1.,-2.42503376499884E-13,0.));
#11015=DIRECTION('',(0.,0.,1.));
#11016=DIRECTION('center_axis',(0.,0.,1.));
#11017=DIRECTION('ref_axis',(1.,-2.42503376499884E-13,0.));
#11018=DIRECTION('',(0.,0.,1.));
#11019=DIRECTION('center_axis',(0.,0.,1.));
#11020=DIRECTION('ref_axis',(1.,-2.42503376499884E-13,0.));
#11021=DIRECTION('',(0.,0.,1.));
#11022=DIRECTION('center_axis',(0.,0.,1.));
#11023=DIRECTION('ref_axis',(1.,-2.42503376499884E-13,0.));
#11024=DIRECTION('',(0.,0.,1.));
#11025=DIRECTION('center_axis',(0.,0.,1.));
#11026=DIRECTION('ref_axis',(1.,-2.42503376499884E-13,0.));
#11027=DIRECTION('',(0.,0.,1.));
#11028=DIRECTION('center_axis',(0.,0.,1.));
#11029=DIRECTION('ref_axis',(1.,-2.42503376499884E-13,0.));
#11030=DIRECTION('',(0.,0.,1.));
#11031=DIRECTION('center_axis',(0.,0.,1.));
#11032=DIRECTION('ref_axis',(1.,-2.42503376499884E-13,0.));
#11033=DIRECTION('',(0.,0.,1.));
#11034=DIRECTION('center_axis',(0.,0.,1.));
#11035=DIRECTION('ref_axis',(1.,-2.42503376499884E-13,0.));
#11036=DIRECTION('',(0.,0.,1.));
#11037=DIRECTION('center_axis',(0.,0.,1.));
#11038=DIRECTION('ref_axis',(1.,-2.42503376499884E-13,0.));
#11039=DIRECTION('',(0.,0.,1.));
#11040=DIRECTION('center_axis',(0.,0.,1.));
#11041=DIRECTION('ref_axis',(1.,-2.42503376499884E-13,0.));
#11042=DIRECTION('',(0.,0.,1.));
#11043=DIRECTION('center_axis',(0.,0.,1.));
#11044=DIRECTION('ref_axis',(1.,-2.42503376499884E-13,0.));
#11045=DIRECTION('',(0.,0.,1.));
#11046=DIRECTION('center_axis',(0.,0.,1.));
#11047=DIRECTION('ref_axis',(1.,-2.42503376499884E-13,0.));
#11048=DIRECTION('',(0.,0.,1.));
#11049=DIRECTION('center_axis',(0.,0.,1.));
#11050=DIRECTION('ref_axis',(1.,-2.42503376499884E-13,0.));
#11051=DIRECTION('',(0.,0.,1.));
#11052=DIRECTION('center_axis',(0.,0.,1.));
#11053=DIRECTION('ref_axis',(1.,-2.42503376499884E-13,0.));
#11054=DIRECTION('',(0.,0.,1.));
#11055=DIRECTION('center_axis',(0.,0.,1.));
#11056=DIRECTION('ref_axis',(1.,-2.42503376499884E-13,0.));
#11057=DIRECTION('',(0.,0.,1.));
#11058=DIRECTION('center_axis',(0.,0.,1.));
#11059=DIRECTION('ref_axis',(1.,-2.42503376499884E-13,0.));
#11060=DIRECTION('',(0.,0.,1.));
#11061=DIRECTION('center_axis',(0.,0.,1.));
#11062=DIRECTION('ref_axis',(1.,-2.42503376499884E-13,0.));
#11063=DIRECTION('',(0.,0.,1.));
#11064=DIRECTION('center_axis',(0.,0.,1.));
#11065=DIRECTION('ref_axis',(1.,-2.42503376499884E-13,0.));
#11066=DIRECTION('',(0.,0.,1.));
#11067=DIRECTION('center_axis',(0.,0.,1.));
#11068=DIRECTION('ref_axis',(1.,-2.42503376499884E-13,0.));
#11069=DIRECTION('',(0.,0.,1.));
#11070=DIRECTION('center_axis',(0.,0.,1.));
#11071=DIRECTION('ref_axis',(1.,-2.42503376499884E-13,0.));
#11072=DIRECTION('',(0.,0.,1.));
#11073=DIRECTION('center_axis',(0.,0.,1.));
#11074=DIRECTION('ref_axis',(1.,-2.42503376499884E-13,0.));
#11075=DIRECTION('',(0.,0.,1.));
#11076=DIRECTION('center_axis',(0.,0.,1.));
#11077=DIRECTION('ref_axis',(1.,-2.42503376499884E-13,0.));
#11078=DIRECTION('',(0.,0.,1.));
#11079=DIRECTION('center_axis',(0.,0.,1.));
#11080=DIRECTION('ref_axis',(1.,-2.42503376499884E-13,0.));
#11081=DIRECTION('',(0.,0.,1.));
#11082=DIRECTION('center_axis',(0.,0.,1.));
#11083=DIRECTION('ref_axis',(1.,-2.42503376499884E-13,0.));
#11084=DIRECTION('',(0.,0.,1.));
#11085=DIRECTION('center_axis',(0.,0.,1.));
#11086=DIRECTION('ref_axis',(1.,-2.42503376499884E-13,0.));
#11087=DIRECTION('',(0.,0.,1.));
#11088=DIRECTION('center_axis',(0.,0.,1.));
#11089=DIRECTION('ref_axis',(1.,-2.42503376499884E-13,0.));
#11090=DIRECTION('',(0.,0.,1.));
#11091=DIRECTION('center_axis',(0.,0.,1.));
#11092=DIRECTION('ref_axis',(1.,-2.42503376499884E-13,0.));
#11093=DIRECTION('',(0.,0.,1.));
#11094=DIRECTION('center_axis',(0.,0.,-1.));
#11095=DIRECTION('ref_axis',(1.,0.,0.));
#11096=DIRECTION('center_axis',(0.,0.,-1.));
#11097=DIRECTION('ref_axis',(1.,0.,0.));
#11098=DIRECTION('',(0.707106781186547,8.65956056235493E-17,0.707106781186548));
#11099=DIRECTION('center_axis',(0.,0.,1.));
#11100=DIRECTION('ref_axis',(1.,0.,0.));
#11101=DIRECTION('center_axis',(0.,0.,1.));
#11102=DIRECTION('ref_axis',(1.,-2.42503376499884E-13,0.));
#11103=DIRECTION('center_axis',(0.,0.,-1.));
#11104=DIRECTION('ref_axis',(1.,-2.42503376499884E-13,0.));
#11105=DIRECTION('center_axis',(0.,0.,1.));
#11106=DIRECTION('ref_axis',(1.,0.,0.));
#11107=DIRECTION('center_axis',(-1.92296268638356E-16,-1.,0.));
#11108=DIRECTION('ref_axis',(1.,-1.92296268638356E-16,0.));
#11109=DIRECTION('',(1.,-1.92296268638356E-16,0.));
#11110=DIRECTION('',(0.,0.,1.));
#11111=DIRECTION('',(1.,-1.92296268638356E-16,0.));
#11112=DIRECTION('',(0.,0.,1.));
#11113=DIRECTION('center_axis',(-0.866025403784439,-0.5,0.));
#11114=DIRECTION('ref_axis',(0.5,-0.866025403784439,0.));
#11115=DIRECTION('',(0.5,-0.866025403784439,0.));
#11116=DIRECTION('',(0.,0.,1.));
#11117=DIRECTION('',(0.5,-0.866025403784439,0.));
#11118=DIRECTION('center_axis',(-0.866025403784439,0.5,0.));
#11119=DIRECTION('ref_axis',(-0.5,-0.866025403784439,0.));
#11120=DIRECTION('',(-0.5,-0.866025403784439,0.));
#11121=DIRECTION('',(0.,0.,1.));
#11122=DIRECTION('',(-0.5,-0.866025403784438,0.));
#11123=DIRECTION('center_axis',(1.92296268638356E-16,1.,0.));
#11124=DIRECTION('ref_axis',(-1.,1.92296268638356E-16,0.));
#11125=DIRECTION('',(-1.,1.92296268638356E-16,0.));
#11126=DIRECTION('',(0.,0.,1.));
#11127=DIRECTION('',(-1.,1.92296268638356E-16,0.));
#11128=DIRECTION('center_axis',(0.866025403784439,0.5,0.));
#11129=DIRECTION('ref_axis',(-0.5,0.866025403784439,0.));
#11130=DIRECTION('',(-0.5,0.866025403784439,0.));
#11131=DIRECTION('',(0.,0.,1.));
#11132=DIRECTION('',(-0.5,0.866025403784439,0.));
#11133=DIRECTION('center_axis',(0.866025403784439,-0.5,0.));
#11134=DIRECTION('ref_axis',(0.5,0.866025403784439,0.));
#11135=DIRECTION('',(0.5,0.866025403784439,0.));
#11136=DIRECTION('',(0.5,0.866025403784439,0.));
#11137=DIRECTION('center_axis',(0.,0.,1.));
#11138=DIRECTION('ref_axis',(1.,0.,0.));
#11139=DIRECTION('center_axis',(0.,0.,1.));
#11140=DIRECTION('ref_axis',(1.,0.,0.));
#11141=DIRECTION('center_axis',(0.,0.,1.));
#11142=DIRECTION('ref_axis',(1.,0.,0.));
#11143=DIRECTION('center_axis',(0.,0.,1.));
#11144=DIRECTION('ref_axis',(1.,0.,0.));
#11145=DIRECTION('',(0.,0.,-1.));
#11146=DIRECTION('center_axis',(0.,0.,1.));
#11147=DIRECTION('ref_axis',(1.,0.,0.));
#11148=DIRECTION('center_axis',(0.,0.,1.));
#11149=DIRECTION('ref_axis',(1.,0.,0.));
#11150=DIRECTION('center_axis',(0.,0.,1.));
#11151=DIRECTION('ref_axis',(1.,0.,0.));
#11152=DIRECTION('axis',(0.,0.,1.));
#11153=DIRECTION('refdir',(1.,0.,0.));
#11154=DIRECTION('center_axis',(0.,0.,-1.));
#11155=DIRECTION('ref_axis',(1.,0.,0.));
#11156=DIRECTION('',(0.,0.,-1.));
#11157=DIRECTION('center_axis',(0.,0.,-1.));
#11158=DIRECTION('ref_axis',(1.,0.,0.));
#11159=DIRECTION('center_axis',(0.,0.,-1.));
#11160=DIRECTION('ref_axis',(1.,0.,0.));
#11161=DIRECTION('',(0.,0.,-1.));
#11162=DIRECTION('center_axis',(0.,0.,-1.));
#11163=DIRECTION('ref_axis',(1.,0.,0.));
#11164=DIRECTION('center_axis',(0.,0.,-1.));
#11165=DIRECTION('ref_axis',(1.,0.,0.));
#11166=DIRECTION('',(0.,0.,-1.));
#11167=DIRECTION('center_axis',(0.,0.,-1.));
#11168=DIRECTION('ref_axis',(1.,0.,0.));
#11169=DIRECTION('',(0.,0.,-1.));
#11170=DIRECTION('center_axis',(0.,0.,-1.));
#11171=DIRECTION('ref_axis',(0.937385399639056,-0.348293859468591,0.));
#11172=DIRECTION('',(0.,0.,-1.));
#11173=DIRECTION('center_axis',(0.,0.,-1.));
#11174=DIRECTION('ref_axis',(1.,0.,0.));
#11175=DIRECTION('center_axis',(0.,0.,-1.));
#11176=DIRECTION('ref_axis',(0.28361887368566,0.958937085782627,0.));
#11177=DIRECTION('',(1.22464679914735E-16,8.07419868282478E-31,-1.));
#11178=DIRECTION('center_axis',(0.,0.,1.));
#11179=DIRECTION('ref_axis',(1.,6.71554824363804E-15,0.));
#11180=DIRECTION('center_axis',(0.,0.,-1.));
#11181=DIRECTION('ref_axis',(1.,6.71554824363804E-15,0.));
#11182=DIRECTION('',(1.22464679914735E-16,8.07419868282478E-31,-1.));
#11183=DIRECTION('center_axis',(0.,0.,-1.));
#11184=DIRECTION('ref_axis',(1.,6.71554824363804E-15,0.));
#11185=DIRECTION('',(1.22464679914735E-16,8.07419868282478E-31,-1.));
#11186=DIRECTION('center_axis',(0.,0.,-1.));
#11187=DIRECTION('ref_axis',(1.,6.71554824363804E-15,0.));
#11188=DIRECTION('',(1.22464679914735E-16,8.07419868282478E-31,-1.));
#11189=DIRECTION('center_axis',(0.,0.,-1.));
#11190=DIRECTION('ref_axis',(-0.60895050335979,-0.793208222636313,0.));
#11191=DIRECTION('',(1.22464679914735E-16,8.07419868282478E-31,-1.));
#11192=DIRECTION('center_axis',(0.,0.,-1.));
#11193=DIRECTION('ref_axis',(1.,6.71554824363804E-15,0.));
#11194=DIRECTION('center_axis',(0.,0.,-1.));
#11195=DIRECTION('ref_axis',(1.,6.71554824363804E-15,0.));
#11196=DIRECTION('center_axis',(0.,0.,1.));
#11197=DIRECTION('ref_axis',(1.,0.,0.));
#11198=DIRECTION('',(0.5,0.866025403784439,0.));
#11199=DIRECTION('',(-0.5,0.866025403784439,0.));
#11200=DIRECTION('',(-1.,0.,0.));
#11201=DIRECTION('',(-0.5,-0.866025403784439,0.));
#11202=DIRECTION('',(0.5,-0.866025403784439,0.));
#11203=DIRECTION('',(1.,-3.49629579342466E-16,0.));
#11204=DIRECTION('center_axis',(0.,0.,-1.));
#11205=DIRECTION('ref_axis',(1.,0.,0.));
#11206=DIRECTION('center_axis',(-3.49629579342466E-16,-1.,0.));
#11207=DIRECTION('ref_axis',(1.,-3.49629579342466E-16,0.));
#11208=DIRECTION('',(1.,-3.49629579342466E-16,0.));
#11209=DIRECTION('',(0.,0.,1.));
#11210=DIRECTION('',(0.,0.,1.));
#11211=DIRECTION('center_axis',(-0.866025403784439,-0.5,0.));
#11212=DIRECTION('ref_axis',(0.5,-0.866025403784439,0.));
#11213=DIRECTION('',(0.5,-0.866025403784439,0.));
#11214=DIRECTION('',(0.,0.,1.));
#11215=DIRECTION('center_axis',(-0.866025403784439,0.5,0.));
#11216=DIRECTION('ref_axis',(-0.5,-0.866025403784439,0.));
#11217=DIRECTION('',(-0.5,-0.866025403784439,0.));
#11218=DIRECTION('',(0.,0.,1.));
#11219=DIRECTION('center_axis',(0.,1.,0.));
#11220=DIRECTION('ref_axis',(-1.,0.,0.));
#11221=DIRECTION('',(-1.,0.,0.));
#11222=DIRECTION('',(0.,0.,1.));
#11223=DIRECTION('center_axis',(0.866025403784439,0.5,0.));
#11224=DIRECTION('ref_axis',(-0.5,0.866025403784439,0.));
#11225=DIRECTION('',(-0.5,0.866025403784439,0.));
#11226=DIRECTION('',(0.,0.,1.));
#11227=DIRECTION('center_axis',(0.866025403784439,-0.5,0.));
#11228=DIRECTION('ref_axis',(0.5,0.866025403784439,0.));
#11229=DIRECTION('',(0.5,0.866025403784439,0.));
#11230=DIRECTION('center_axis',(0.,0.,1.));
#11231=DIRECTION('ref_axis',(1.,0.,0.));
#11232=DIRECTION('axis',(0.,0.,1.));
#11233=DIRECTION('refdir',(1.,0.,0.));
#11234=DIRECTION('center_axis',(0.,0.,-1.));
#11235=DIRECTION('ref_axis',(1.,0.,0.));
#11236=DIRECTION('center_axis',(1.16928610669829E-31,-5.97538301968883E-32,
-1.));
#11237=DIRECTION('ref_axis',(1.,0.,0.));
#11238=DIRECTION('',(0.,0.,-1.));
#11239=DIRECTION('center_axis',(-6.45616000593692E-32,-1.81182428107391E-19,
1.));
#11240=DIRECTION('ref_axis',(1.,0.,0.));
#11241=DIRECTION('center_axis',(0.,0.,-1.));
#11242=DIRECTION('ref_axis',(1.,0.,0.));
#11243=DIRECTION('center_axis',(1.16928610669829E-31,-5.97538301968883E-32,
-1.));
#11244=DIRECTION('ref_axis',(1.,0.,0.));
#11245=DIRECTION('',(0.,0.,-1.));
#11246=DIRECTION('center_axis',(-6.45616000593692E-32,-1.81182428107391E-19,
1.));
#11247=DIRECTION('ref_axis',(1.,0.,0.));
#11248=DIRECTION('center_axis',(0.,0.,1.));
#11249=DIRECTION('ref_axis',(1.,0.,0.));
#11250=DIRECTION('center_axis',(0.,0.,1.));
#11251=DIRECTION('ref_axis',(1.,0.,0.));
#11252=DIRECTION('center_axis',(0.,0.,-1.));
#11253=DIRECTION('ref_axis',(1.,0.,0.));
#11254=DIRECTION('center_axis',(0.,0.,-1.));
#11255=DIRECTION('ref_axis',(1.,0.,0.));
#11256=DIRECTION('center_axis',(0.,0.,-1.));
#11257=DIRECTION('ref_axis',(1.,0.,0.));
#11258=DIRECTION('',(0.,0.,1.));
#11259=DIRECTION('center_axis',(0.,0.,1.));
#11260=DIRECTION('ref_axis',(1.,0.,0.));
#11261=DIRECTION('center_axis',(0.,0.,1.));
#11262=DIRECTION('ref_axis',(1.,0.,0.));
#11263=DIRECTION('center_axis',(0.,0.,1.));
#11264=DIRECTION('ref_axis',(1.,0.,0.));
#11265=DIRECTION('center_axis',(0.,0.,-1.));
#11266=DIRECTION('ref_axis',(1.,0.,0.));
#11267=DIRECTION('center_axis',(0.,0.,-1.));
#11268=DIRECTION('ref_axis',(1.,0.,0.));
#11269=DIRECTION('center_axis',(0.,0.,-1.));
#11270=DIRECTION('ref_axis',(1.,0.,0.));
#11271=DIRECTION('',(0.,0.,1.));
#11272=DIRECTION('center_axis',(0.,0.,1.));
#11273=DIRECTION('ref_axis',(1.,0.,0.));
#11274=DIRECTION('center_axis',(0.,0.,1.));
#11275=DIRECTION('ref_axis',(1.,0.,0.));
#11276=DIRECTION('center_axis',(0.,0.,1.));
#11277=DIRECTION('ref_axis',(1.,0.,0.));
#11278=DIRECTION('center_axis',(0.,0.,-1.));
#11279=DIRECTION('ref_axis',(1.,0.,0.));
#11280=DIRECTION('center_axis',(0.,0.,-1.));
#11281=DIRECTION('ref_axis',(1.,0.,0.));
#11282=DIRECTION('center_axis',(0.,0.,-1.));
#11283=DIRECTION('ref_axis',(1.,0.,0.));
#11284=DIRECTION('',(0.,0.,1.));
#11285=DIRECTION('center_axis',(0.,0.,1.));
#11286=DIRECTION('ref_axis',(1.,0.,0.));
#11287=DIRECTION('center_axis',(0.,0.,1.));
#11288=DIRECTION('ref_axis',(1.,0.,0.));
#11289=DIRECTION('center_axis',(0.,0.,1.));
#11290=DIRECTION('ref_axis',(1.,0.,0.));
#11291=DIRECTION('center_axis',(0.,0.,-1.));
#11292=DIRECTION('ref_axis',(1.,0.,0.));
#11293=DIRECTION('center_axis',(0.,0.,-1.));
#11294=DIRECTION('ref_axis',(1.,0.,0.));
#11295=DIRECTION('center_axis',(0.,0.,-1.));
#11296=DIRECTION('ref_axis',(1.,0.,0.));
#11297=DIRECTION('',(0.,0.,1.));
#11298=DIRECTION('center_axis',(0.,0.,1.));
#11299=DIRECTION('ref_axis',(1.,0.,0.));
#11300=DIRECTION('center_axis',(0.,0.,-1.));
#11301=DIRECTION('ref_axis',(1.,0.,0.));
#11302=DIRECTION('',(0.,0.,1.));
#11303=DIRECTION('center_axis',(-6.45616000593692E-32,-1.81182428107391E-19,
1.));
#11304=DIRECTION('ref_axis',(1.,0.,0.));
#11305=DIRECTION('center_axis',(0.,0.,-1.));
#11306=DIRECTION('ref_axis',(1.,0.,0.));
#11307=DIRECTION('',(0.,0.,1.));
#11308=DIRECTION('center_axis',(-6.45616000593692E-32,-1.81182428107391E-19,
1.));
#11309=DIRECTION('ref_axis',(1.,0.,0.));
#11310=DIRECTION('center_axis',(0.,0.,-1.));
#11311=DIRECTION('ref_axis',(1.,0.,0.));
#11312=DIRECTION('',(0.,0.,1.));
#11313=DIRECTION('center_axis',(-6.45616000593692E-32,-1.81182428107391E-19,
1.));
#11314=DIRECTION('ref_axis',(1.,0.,0.));
#11315=DIRECTION('center_axis',(0.,0.,-1.));
#11316=DIRECTION('ref_axis',(1.,0.,0.));
#11317=DIRECTION('',(0.,0.,1.));
#11318=DIRECTION('center_axis',(-6.45616000593692E-32,-1.81182428107391E-19,
1.));
#11319=DIRECTION('ref_axis',(1.,0.,0.));
#11320=DIRECTION('center_axis',(0.,1.,0.));
#11321=DIRECTION('ref_axis',(0.,0.,1.));
#11322=DIRECTION('center_axis',(0.998287351281347,-0.0585009766728139,0.));
#11323=DIRECTION('ref_axis',(0.0584117362954384,0.996764512774636,0.0552139034672828));
#11324=DIRECTION('center_axis',(-3.13156554427463E-33,-1.,5.97538301968883E-32));
#11325=DIRECTION('ref_axis',(0.688354575693766,0.,0.725374371012276));
#11326=DIRECTION('center_axis',(1.38968329343724E-15,1.,0.));
#11327=DIRECTION('ref_axis',(0.,0.,1.));
#11328=DIRECTION('',(3.13156554427463E-33,1.,-5.97538301968883E-32));
#11329=DIRECTION('',(-3.13156554427463E-33,-1.,5.97538301968883E-32));
#11330=DIRECTION('center_axis',(0.998287351281345,0.0585009766728351,0.));
#11331=DIRECTION('ref_axis',(0.,0.,1.));
#11332=DIRECTION('center_axis',(0.996325437245183,-0.0856482521607663,0.));
#11333=DIRECTION('ref_axis',(0.,0.,1.));
#11334=DIRECTION('center_axis',(-1.38968329343725E-15,-1.,-6.75000545323542E-30));
#11335=DIRECTION('ref_axis',(-4.85722573273506E-15,0.,1.));
#11336=DIRECTION('center_axis',(-3.13156554427485E-33,1.,-5.97538301968883E-32));
#11337=DIRECTION('ref_axis',(-0.688354575693752,0.,0.72537437101229));
#11338=DIRECTION('center_axis',(1.38968329343726E-15,-1.,0.));
#11339=DIRECTION('ref_axis',(0.,0.,1.));
#11340=DIRECTION('',(3.13156554427485E-33,-1.,5.97538301968883E-32));
#11341=DIRECTION('',(-3.13156554427485E-33,1.,-5.97538301968883E-32));
#11342=DIRECTION('center_axis',(-0.996325437245184,-0.0856482521607654,
-4.83937755196581E-15));
#11343=DIRECTION('ref_axis',(-4.85722573273506E-15,0.,1.));
#11344=DIRECTION('center_axis',(0.998629534754574,0.,-0.0523359562429439));
#11345=DIRECTION('ref_axis',(-0.0523359562429439,0.,-0.998629534754574));
#11346=DIRECTION('',(0.,1.,0.));
#11347=DIRECTION('center_axis',(-1.16928610669829E-31,5.97538301968883E-32,
1.));
#11348=DIRECTION('ref_axis',(1.,0.,1.16928610669829E-31));
#11349=DIRECTION('center_axis',(-0.998629534754574,0.,-0.0523359562429402));
#11350=DIRECTION('ref_axis',(-0.0523359562429402,0.,0.998629534754574));
#11351=DIRECTION('',(0.,-1.,0.));
#11352=DIRECTION('center_axis',(-6.45616000593692E-32,-1.81182428107391E-19,
1.));
#11353=DIRECTION('ref_axis',(1.,0.,6.45616000593692E-32));
#11354=DIRECTION('',(0.,0.,1.));
#11355=DIRECTION('',(1.,0.,0.));
#11356=DIRECTION('',(0.,-1.22464679914735E-16,-1.));
#11357=DIRECTION('',(1.,0.,0.));
#11358=DIRECTION('',(0.,-1.22464679914735E-16,-1.));
#11359=DIRECTION('',(1.,0.,0.));
#11360=DIRECTION('',(0.,0.,1.));
#11361=DIRECTION('',(1.,0.,0.));
#11362=DIRECTION('',(0.,0.,1.));
#11363=DIRECTION('',(1.,0.,0.));
#11364=DIRECTION('',(0.,-1.22464679914735E-16,-1.));
#11365=DIRECTION('',(1.,0.,0.));
#11366=DIRECTION('',(0.,0.,1.));
#11367=DIRECTION('',(1.,0.,0.));
#11368=DIRECTION('',(0.,-1.22464679914735E-16,-1.));
#11369=DIRECTION('',(1.,0.,0.));
#11370=DIRECTION('axis',(0.,0.,1.));
#11371=DIRECTION('refdir',(1.,0.,0.));
#11372=DIRECTION('center_axis',(0.,0.,1.));
#11373=DIRECTION('ref_axis',(1.,0.,0.));
#11374=DIRECTION('center_axis',(0.,0.,-1.));
#11375=DIRECTION('ref_axis',(1.,0.,0.));
#11376=DIRECTION('',(0.,0.,-1.));
#11377=DIRECTION('center_axis',(0.,0.,-1.));
#11378=DIRECTION('ref_axis',(1.,0.,0.));
#11379=DIRECTION('center_axis',(0.,0.,1.));
#11380=DIRECTION('ref_axis',(1.,0.,0.));
#11381=DIRECTION('center_axis',(0.,0.,1.));
#11382=DIRECTION('ref_axis',(1.,0.,0.));
#11383=DIRECTION('',(0.,0.,-1.));
#11384=DIRECTION('center_axis',(0.,0.,1.));
#11385=DIRECTION('ref_axis',(1.,0.,0.));
#11386=DIRECTION('center_axis',(0.,0.,1.));
#11387=DIRECTION('ref_axis',(1.,0.,0.));
#11388=DIRECTION('center_axis',(0.,0.,1.));
#11389=DIRECTION('ref_axis',(1.,0.,0.));
#11390=DIRECTION('',(0.,0.,1.));
#11391=DIRECTION('',(1.,0.,0.));
#11392=DIRECTION('',(0.,0.,1.));
#11393=DIRECTION('',(1.,0.,0.));
#11394=DIRECTION('',(-9.47648575109602E-18,-1.10990672499979E-16,-1.));
#11395=DIRECTION('',(0.906307619284642,0.422618621485853,-5.54953362499899E-17));
#11396=DIRECTION('',(0.,0.,1.));
#11397=DIRECTION('',(1.,0.,0.));
#11398=DIRECTION('',(0.,0.,1.));
#11399=DIRECTION('',(1.,0.,0.));
#11400=DIRECTION('',(0.,0.,1.));
#11401=DIRECTION('',(1.,0.,0.));
#11402=DIRECTION('',(-9.47648575109602E-18,-1.10990672499979E-16,-1.));
#11403=DIRECTION('',(0.906307619284642,0.422618621485853,-5.54953362499899E-17));
#11404=DIRECTION('',(0.,0.,1.));
#11405=DIRECTION('',(1.,0.,0.));
#11406=CARTESIAN_POINT('',(0.,0.,0.));
#11407=CARTESIAN_POINT('',(0.,0.,0.));
#11408=CARTESIAN_POINT('Origin',(6.,-2.5,0.3));
#11409=CARTESIAN_POINT('',(5.83,-2.5,0.6));
#11410=CARTESIAN_POINT('Origin',(6.,-2.5,0.6));
#11411=CARTESIAN_POINT('',(5.83,-2.5,0.));
#11412=CARTESIAN_POINT('',(5.83,-2.5,0.3));
#11413=CARTESIAN_POINT('Origin',(6.,-2.5,0.));
#11414=CARTESIAN_POINT('Origin',(12.8,-2.5,0.3));
#11415=CARTESIAN_POINT('',(12.63,-2.5,0.6));
#11416=CARTESIAN_POINT('Origin',(12.8,-2.5,0.6));
#11417=CARTESIAN_POINT('',(12.63,-2.5,0.));
#11418=CARTESIAN_POINT('',(12.63,-2.5,0.3));
#11419=CARTESIAN_POINT('Origin',(12.8,-2.5,0.));
#11420=CARTESIAN_POINT('Origin',(0.,0.,0.3));
#11421=CARTESIAN_POINT('',(-0.41,5.02105187650415E-17,0.6));
#11422=CARTESIAN_POINT('Origin',(0.,0.,0.6));
#11423=CARTESIAN_POINT('',(-0.41,5.02105187650415E-17,0.));
#11424=CARTESIAN_POINT('',(-0.41,5.02105187650415E-17,0.3));
#11425=CARTESIAN_POINT('Origin',(0.,0.,0.));
#11426=CARTESIAN_POINT('Origin',(-3.,0.08,0.6));
#11427=CARTESIAN_POINT('',(-2.94222222222222,0.,0.6));
#11428=CARTESIAN_POINT('',(-2.94222222222222,0.,-0.3));
#11429=CARTESIAN_POINT('',(-2.94222222222222,-2.22044604925031E-16,0.3));
#11430=CARTESIAN_POINT('',(-3.,0.08,0.6));
#11431=CARTESIAN_POINT('',(-2.4668154158215,-0.658255578093306,0.6));
#11432=CARTESIAN_POINT('',(-3.,0.08,-0.3));
#11433=CARTESIAN_POINT('',(-3.,0.08,0.6));
#11434=CARTESIAN_POINT('',(-3.62244421906694,0.94184584178499,-0.3));
#11435=CARTESIAN_POINT('Origin',(-3.065,-0.01,0.6));
#11436=CARTESIAN_POINT('',(-3.05777777777778,0.,-0.3));
#11437=CARTESIAN_POINT('',(-3.05777777777778,0.,0.6));
#11438=CARTESIAN_POINT('',(-3.05777777777778,4.44089209850063E-16,0.3));
#11439=CARTESIAN_POINT('',(-3.45559330628803,-0.550821501014198,-0.3));
#11440=CARTESIAN_POINT('',(-2.53728701825558,0.720679513184584,0.6));
#11441=CARTESIAN_POINT('Origin',(-3.4,0.08,0.6));
#11442=CARTESIAN_POINT('',(-3.34222222222222,0.,0.6));
#11443=CARTESIAN_POINT('',(-3.34222222222222,0.,-0.3));
#11444=CARTESIAN_POINT('',(-3.34222222222222,-2.22044604925031E-16,0.3));
#11445=CARTESIAN_POINT('',(-3.4,0.08,0.6));
#11446=CARTESIAN_POINT('',(-2.79825557809331,-0.753184584178499,0.6));
#11447=CARTESIAN_POINT('',(-3.4,0.08,-0.3));
#11448=CARTESIAN_POINT('',(-3.4,0.08,0.6));
#11449=CARTESIAN_POINT('',(-3.95388438133874,0.846916835699797,-0.3));
#11450=CARTESIAN_POINT('Origin',(-3.465,-0.01,0.6));
#11451=CARTESIAN_POINT('',(-3.45777777777778,0.,-0.3));
#11452=CARTESIAN_POINT('',(-3.45777777777778,0.,0.6));
#11453=CARTESIAN_POINT('',(-3.45777777777778,2.22044604925031E-16,0.3));
#11454=CARTESIAN_POINT('',(-3.78703346855984,-0.455892494929006,-0.3));
#11455=CARTESIAN_POINT('',(-2.86872718052738,0.815608519269777,0.6));
#11456=CARTESIAN_POINT('Origin',(-3.8,0.08,0.6));
#11457=CARTESIAN_POINT('',(-3.74222222222222,0.,0.6));
#11458=CARTESIAN_POINT('',(-3.74222222222222,0.,-0.3));
#11459=CARTESIAN_POINT('',(-3.74222222222222,2.22044604925031E-16,0.3));
#11460=CARTESIAN_POINT('',(-3.8,0.08,0.6));
#11461=CARTESIAN_POINT('',(-3.12969574036512,-0.84811359026369,0.6));
#11462=CARTESIAN_POINT('',(-3.8,0.08,-0.3));
#11463=CARTESIAN_POINT('',(-3.8,0.08,0.6));
#11464=CARTESIAN_POINT('',(-4.28532454361054,0.751987829614604,-0.3));
#11465=CARTESIAN_POINT('Origin',(-3.865,-0.01,0.6));
#11466=CARTESIAN_POINT('',(-3.85777777777778,0.,-0.3));
#11467=CARTESIAN_POINT('',(-3.85777777777778,0.,0.6));
#11468=CARTESIAN_POINT('',(-3.85777777777778,4.44089209850063E-16,0.3));
#11469=CARTESIAN_POINT('',(-4.11847363083164,-0.360963488843813,-0.3));
#11470=CARTESIAN_POINT('',(-3.20016734279919,0.910537525354969,0.6));
#11471=CARTESIAN_POINT('Origin',(-4.2,0.08,0.6));
#11472=CARTESIAN_POINT('',(-4.14222222222222,0.,0.6));
#11473=CARTESIAN_POINT('',(-4.14222222222222,0.,-0.3));
#11474=CARTESIAN_POINT('',(-4.14222222222222,0.,0.3));
#11475=CARTESIAN_POINT('',(-4.2,0.08,0.6));
#11476=CARTESIAN_POINT('',(-3.46113590263691,-0.943042596348886,0.6));
#11477=CARTESIAN_POINT('',(-4.2,0.08,-0.3));
#11478=CARTESIAN_POINT('',(-4.2,0.08,0.6));
#11479=CARTESIAN_POINT('',(-4.61676470588236,0.657058823529412,-0.3));
#11480=CARTESIAN_POINT('Origin',(-4.265,-0.01,0.6));
#11481=CARTESIAN_POINT('',(-4.25777777777778,0.,-0.3));
#11482=CARTESIAN_POINT('',(-4.25777777777778,0.,0.6));
#11483=CARTESIAN_POINT('',(-4.25777777777778,-2.22044604925031E-16,0.3));
#11484=CARTESIAN_POINT('',(-4.44991379310344,-0.266034482758619,-0.3));
#11485=CARTESIAN_POINT('',(-3.531607505071,1.00546653144016,0.6));
#11486=CARTESIAN_POINT('Origin',(-4.6,0.08,0.6));
#11487=CARTESIAN_POINT('',(-4.54222222222222,0.,0.6));
#11488=CARTESIAN_POINT('',(-4.54222222222222,0.,-0.3));
#11489=CARTESIAN_POINT('',(-4.54222222222222,2.22044604925031E-16,0.3));
#11490=CARTESIAN_POINT('',(-4.6,0.08,0.6));
#11491=CARTESIAN_POINT('',(-3.79257606490873,-1.03797160243407,0.6));
#11492=CARTESIAN_POINT('',(-4.6,0.08,-0.3));
#11493=CARTESIAN_POINT('',(-4.6,0.08,0.6));
#11494=CARTESIAN_POINT('',(-4.94820486815415,0.562129817444219,-0.3));
#11495=CARTESIAN_POINT('Origin',(-4.665,-0.01,0.6));
#11496=CARTESIAN_POINT('',(-4.65777777777778,0.,-0.3));
#11497=CARTESIAN_POINT('',(-4.65777777777778,0.,0.6));
#11498=CARTESIAN_POINT('',(-4.65777777777778,0.,0.3));
#11499=CARTESIAN_POINT('',(-4.78135395537526,-0.171105476673429,-0.3));
#11500=CARTESIAN_POINT('',(-3.86304766734279,1.10039553752536,0.6));
#11501=CARTESIAN_POINT('Origin',(-5.,0.08,0.6));
#11502=CARTESIAN_POINT('',(-4.94222222222222,0.,0.6));
#11503=CARTESIAN_POINT('',(-4.94222222222222,0.,-0.3));
#11504=CARTESIAN_POINT('',(-4.94222222222222,0.,0.3));
#11505=CARTESIAN_POINT('',(-5.,0.08,0.6));
#11506=CARTESIAN_POINT('',(-4.12401622718054,-1.13290060851927,0.6));
#11507=CARTESIAN_POINT('',(-5.,0.08,-0.3));
#11508=CARTESIAN_POINT('',(-5.,0.08,0.6));
#11509=CARTESIAN_POINT('',(-5.27964503042596,0.467200811359026,-0.3));
#11510=CARTESIAN_POINT('Origin',(-5.065,-0.01,0.6));
#11511=CARTESIAN_POINT('',(-5.05777777777778,0.,-0.3));
#11512=CARTESIAN_POINT('',(-5.05777777777778,0.,0.6));
#11513=CARTESIAN_POINT('',(-5.05777777777778,-2.22044604925031E-16,0.3));
#11514=CARTESIAN_POINT('',(-5.11279411764706,-0.076176470588234,-0.3));
#11515=CARTESIAN_POINT('',(-4.19448782961461,1.19532454361054,0.6));
#11516=CARTESIAN_POINT('Origin',(-5.4,0.08,0.6));
#11517=CARTESIAN_POINT('',(-5.34222222222222,0.,0.6));
#11518=CARTESIAN_POINT('',(-5.34222222222222,0.,-0.3));
#11519=CARTESIAN_POINT('',(-5.34222222222222,0.,0.3));
#11520=CARTESIAN_POINT('',(-5.4,0.08,0.6));
#11521=CARTESIAN_POINT('',(-4.45545638945233,-1.22782961460446,0.6));
#11522=CARTESIAN_POINT('',(-5.4,0.08,-0.3));
#11523=CARTESIAN_POINT('',(-5.4,0.08,0.6));
#11524=CARTESIAN_POINT('',(-5.61108519269777,0.372271805273833,-0.3));
#11525=CARTESIAN_POINT('Origin',(-5.465,-0.01,0.6));
#11526=CARTESIAN_POINT('',(-5.45777777777778,0.,-0.3));
#11527=CARTESIAN_POINT('',(-5.45777777777778,0.,0.6));
#11528=CARTESIAN_POINT('',(-5.45777777777778,-2.22044604925031E-16,0.3));
#11529=CARTESIAN_POINT('',(-5.44423427991886,0.0187525354969586,-0.3));
#11530=CARTESIAN_POINT('',(-4.52592799188642,1.29025354969574,0.6));
#11531=CARTESIAN_POINT('Origin',(-5.8,0.08,0.6));
#11532=CARTESIAN_POINT('',(-5.74222222222222,0.,0.6));
#11533=CARTESIAN_POINT('',(-5.74222222222222,0.,-0.3));
#11534=CARTESIAN_POINT('',(-5.74222222222222,2.22044604925031E-16,0.3));
#11535=CARTESIAN_POINT('',(-5.8,0.08,0.6));
#11536=CARTESIAN_POINT('',(-4.78689655172415,-1.32275862068965,0.6));
#11537=CARTESIAN_POINT('',(-5.8,0.08,-0.3));
#11538=CARTESIAN_POINT('',(-5.8,0.08,0.6));
#11539=CARTESIAN_POINT('',(-5.94252535496957,0.277342799188642,-0.3));
#11540=CARTESIAN_POINT('Origin',(-5.865,-0.01,0.6));
#11541=CARTESIAN_POINT('',(-5.85777777777778,0.,-0.3));
#11542=CARTESIAN_POINT('',(-5.85777777777778,0.,0.6));
#11543=CARTESIAN_POINT('',(-5.85777777777778,0.,0.3));
#11544=CARTESIAN_POINT('',(-5.77567444219067,0.113681541582149,-0.3));
#11545=CARTESIAN_POINT('',(-4.85736815415821,1.38518255578094,0.6));
#11546=CARTESIAN_POINT('Origin',(-6.2,0.08,0.6));
#11547=CARTESIAN_POINT('',(-6.14222222222222,0.,0.6));
#11548=CARTESIAN_POINT('',(-6.14222222222222,0.,-0.3));
#11549=CARTESIAN_POINT('',(-6.14222222222222,2.22044604925031E-16,0.3));
#11550=CARTESIAN_POINT('',(-6.2,0.08,0.6));
#11551=CARTESIAN_POINT('',(-5.11833671399593,-1.41768762677485,0.6));
#11552=CARTESIAN_POINT('',(-6.2,0.08,-0.3));
#11553=CARTESIAN_POINT('',(-6.2,0.08,0.6));
#11554=CARTESIAN_POINT('',(-6.27396551724138,0.182413793103448,-0.3));
#11555=CARTESIAN_POINT('Origin',(-6.265,-0.01,0.6));
#11556=CARTESIAN_POINT('',(-6.25777777777778,0.,-0.3));
#11557=CARTESIAN_POINT('',(-6.25777777777778,0.,0.6));
#11558=CARTESIAN_POINT('',(-6.25777777777778,-2.22044604925031E-16,0.3));
#11559=CARTESIAN_POINT('',(-6.10711460446247,0.208610547667344,-0.3));
#11560=CARTESIAN_POINT('',(-5.18880831643003,1.48011156186612,0.6));
#11561=CARTESIAN_POINT('Origin',(-10.2,0.08,0.6));
#11562=CARTESIAN_POINT('',(-10.1422222222222,0.,0.6));
#11563=CARTESIAN_POINT('',(-10.1422222222222,0.,-0.3));
#11564=CARTESIAN_POINT('',(-10.1422222222222,1.38777878078145E-17,0.3));
#11565=CARTESIAN_POINT('',(-10.2,0.08,0.6));
#11566=CARTESIAN_POINT('',(-8.43273833671401,-2.36697768762677,0.6));
#11567=CARTESIAN_POINT('',(-10.2,0.08,-0.3));
#11568=CARTESIAN_POINT('',(-10.2,0.08,0.6));
#11569=CARTESIAN_POINT('',(-9.58836713995944,-0.766876267748476,-0.3));
#11570=CARTESIAN_POINT('Origin',(-10.265,-0.01,0.6));
#11571=CARTESIAN_POINT('',(-10.2577777777778,0.,-0.3));
#11572=CARTESIAN_POINT('',(-10.2577777777778,0.,0.6));
#11573=CARTESIAN_POINT('',(-10.2577777777778,6.93889390390723E-18,0.3));
#11574=CARTESIAN_POINT('',(-9.42151622718051,1.15790060851927,-0.3));
#11575=CARTESIAN_POINT('',(-8.50320993914803,2.42940162271807,0.6));
#11576=CARTESIAN_POINT('Origin',(-6.8,0.08,0.6));
#11577=CARTESIAN_POINT('',(-6.74222222222222,0.,0.6));
#11578=CARTESIAN_POINT('',(-6.74222222222222,0.,-0.3));
#11579=CARTESIAN_POINT('',(-6.74222222222222,1.11022302462516E-16,0.3));
#11580=CARTESIAN_POINT('',(-6.8,0.08,0.6));
#11581=CARTESIAN_POINT('',(-5.61549695740364,-1.56008113590264,0.6));
#11582=CARTESIAN_POINT('',(-6.8,0.08,-0.3));
#11583=CARTESIAN_POINT('',(-6.8,0.08,0.6));
#11584=CARTESIAN_POINT('',(-6.77112576064909,0.0400202839756583,-0.3));
#11585=CARTESIAN_POINT('Origin',(-6.865,-0.01,0.6));
#11586=CARTESIAN_POINT('',(-6.85777777777778,0.,-0.3));
#11587=CARTESIAN_POINT('',(-6.85777777777778,0.,0.6));
#11588=CARTESIAN_POINT('',(-6.85777777777778,1.11022302462516E-16,0.3));
#11589=CARTESIAN_POINT('',(-6.60427484787018,0.351004056795132,-0.3));
#11590=CARTESIAN_POINT('',(-5.68596855983772,1.62250507099392,0.6));
#11591=CARTESIAN_POINT('Origin',(-7.2,0.08,0.6));
#11592=CARTESIAN_POINT('',(-7.14222222222222,0.,0.6));
#11593=CARTESIAN_POINT('',(-7.14222222222222,0.,-0.3));
#11594=CARTESIAN_POINT('',(-7.14222222222222,1.11022302462516E-16,0.3));
#11595=CARTESIAN_POINT('',(-7.2,0.08,0.6));
#11596=CARTESIAN_POINT('',(-5.94693711967545,-1.65501014198783,0.6));
#11597=CARTESIAN_POINT('',(-7.2,0.08,-0.3));
#11598=CARTESIAN_POINT('',(-7.2,0.08,0.6));
#11599=CARTESIAN_POINT('',(-7.10256592292089,-0.0549087221095346,-0.3));
#11600=CARTESIAN_POINT('Origin',(-7.265,-0.01,0.6));
#11601=CARTESIAN_POINT('',(-7.25777777777778,0.,-0.3));
#11602=CARTESIAN_POINT('',(-7.25777777777778,0.,0.6));
#11603=CARTESIAN_POINT('',(-7.25777777777778,1.11022302462516E-16,0.3));
#11604=CARTESIAN_POINT('',(-6.93571501014199,0.445933062880325,-0.3));
#11605=CARTESIAN_POINT('',(-6.01740872210952,1.71743407707911,0.6));
#11606=CARTESIAN_POINT('Origin',(-7.6,0.08,0.6));
#11607=CARTESIAN_POINT('',(-7.54222222222222,0.,0.6));
#11608=CARTESIAN_POINT('',(-7.54222222222222,0.,-0.3));
#11609=CARTESIAN_POINT('',(-7.54222222222222,0.,0.3));
#11610=CARTESIAN_POINT('',(-7.6,0.08,0.6));
#11611=CARTESIAN_POINT('',(-6.27837728194725,-1.74993914807303,0.6));
#11612=CARTESIAN_POINT('',(-7.6,0.08,-0.3));
#11613=CARTESIAN_POINT('',(-7.6,0.08,0.6));
#11614=CARTESIAN_POINT('',(-7.43400608519269,-0.149837728194727,-0.3));
#11615=CARTESIAN_POINT('Origin',(-7.665,-0.01,0.6));
#11616=CARTESIAN_POINT('',(-7.65777777777778,0.,-0.3));
#11617=CARTESIAN_POINT('',(-7.65777777777778,0.,0.6));
#11618=CARTESIAN_POINT('',(-7.65777777777778,1.11022302462516E-16,0.3));
#11619=CARTESIAN_POINT('',(-7.26715517241379,0.540862068965518,-0.3));
#11620=CARTESIAN_POINT('',(-6.34884888438131,1.81236308316431,0.6));
#11621=CARTESIAN_POINT('Origin',(-8.,0.08,0.6));
#11622=CARTESIAN_POINT('',(-7.94222222222222,0.,0.6));
#11623=CARTESIAN_POINT('',(-7.94222222222222,0.,-0.3));
#11624=CARTESIAN_POINT('',(-7.94222222222222,0.,0.3));
#11625=CARTESIAN_POINT('',(-8.,0.08,0.6));
#11626=CARTESIAN_POINT('',(-6.60981744421906,-1.84486815415822,0.6));
#11627=CARTESIAN_POINT('',(-8.,0.08,-0.3));
#11628=CARTESIAN_POINT('',(-8.,0.08,0.6));
#11629=CARTESIAN_POINT('',(-7.7654462474645,-0.24476673427992,-0.3));
#11630=CARTESIAN_POINT('Origin',(-8.065,-0.01,0.6));
#11631=CARTESIAN_POINT('',(-8.05777777777778,0.,-0.3));
#11632=CARTESIAN_POINT('',(-8.05777777777778,0.,0.6));
#11633=CARTESIAN_POINT('',(-8.05777777777778,1.11022302462516E-16,0.3));
#11634=CARTESIAN_POINT('',(-7.59859533468559,0.635791075050711,-0.3));
#11635=CARTESIAN_POINT('',(-6.68028904665311,1.90729208924951,0.6));
#11636=CARTESIAN_POINT('Origin',(-8.4,0.08,0.6));
#11637=CARTESIAN_POINT('',(-8.34222222222222,0.,0.6));
#11638=CARTESIAN_POINT('',(-8.34222222222222,0.,-0.3));
#11639=CARTESIAN_POINT('',(-8.34222222222222,0.,0.3));
#11640=CARTESIAN_POINT('',(-8.4,0.08,0.6));
#11641=CARTESIAN_POINT('',(-6.94125760649083,-1.93979716024342,0.6));
#11642=CARTESIAN_POINT('',(-8.4,0.08,-0.3));
#11643=CARTESIAN_POINT('',(-8.4,0.08,0.6));
#11644=CARTESIAN_POINT('',(-8.0968864097363,-0.339695740365117,-0.3));
#11645=CARTESIAN_POINT('Origin',(-8.465,-0.01,0.6));
#11646=CARTESIAN_POINT('',(-8.45777777777778,0.,-0.3));
#11647=CARTESIAN_POINT('',(-8.45777777777778,0.,0.6));
#11648=CARTESIAN_POINT('',(-8.45777777777778,0.,0.3));
#11649=CARTESIAN_POINT('',(-7.93003549695741,0.730720081135902,-0.3));
#11650=CARTESIAN_POINT('',(-7.01172920892496,2.00222109533468,0.6));
#11651=CARTESIAN_POINT('Origin',(-8.8,0.08,0.6));
#11652=CARTESIAN_POINT('',(-8.74222222222222,0.,0.6));
#11653=CARTESIAN_POINT('',(-8.74222222222222,0.,-0.3));
#11654=CARTESIAN_POINT('',(-8.74222222222222,0.,0.3));
#11655=CARTESIAN_POINT('',(-8.8,0.08,0.6));
#11656=CARTESIAN_POINT('',(-7.27269776876264,-2.03472616632861,0.6));
#11657=CARTESIAN_POINT('',(-8.8,0.08,-0.3));
#11658=CARTESIAN_POINT('',(-8.8,0.08,0.6));
#11659=CARTESIAN_POINT('',(-8.4283265720081,-0.43462474645031,-0.3));
#11660=CARTESIAN_POINT('Origin',(-8.865,-0.01,0.6));
#11661=CARTESIAN_POINT('',(-8.85777777777778,0.,-0.3));
#11662=CARTESIAN_POINT('',(-8.85777777777778,0.,0.6));
#11663=CARTESIAN_POINT('',(-8.85777777777778,-5.55111512312578E-17,0.3));
#11664=CARTESIAN_POINT('',(-8.26147565922921,0.825649087221095,-0.3));
#11665=CARTESIAN_POINT('',(-7.34316937119677,2.09715010141987,0.6));
#11666=CARTESIAN_POINT('Origin',(-9.2,0.08,0.6));
#11667=CARTESIAN_POINT('',(-9.14222222222222,0.,0.6));
#11668=CARTESIAN_POINT('',(-9.14222222222222,0.,-0.3));
#11669=CARTESIAN_POINT('',(-9.14222222222222,0.,0.3));
#11670=CARTESIAN_POINT('',(-9.2,0.08,0.6));
#11671=CARTESIAN_POINT('',(-7.6041379310345,-2.12965517241379,0.6));
#11672=CARTESIAN_POINT('',(-9.2,0.08,-0.3));
#11673=CARTESIAN_POINT('',(-9.2,0.08,0.6));
#11674=CARTESIAN_POINT('',(-8.75976673427992,-0.529553752535495,-0.3));
#11675=CARTESIAN_POINT('Origin',(-9.265,-0.01,0.6));
#11676=CARTESIAN_POINT('',(-9.25777777777778,0.,-0.3));
#11677=CARTESIAN_POINT('',(-9.25777777777778,0.,0.6));
#11678=CARTESIAN_POINT('',(-9.25777777777778,0.,0.3));
#11679=CARTESIAN_POINT('',(-8.592915821501,0.920578093306291,-0.3));
#11680=CARTESIAN_POINT('',(-7.67460953346852,2.19207910750508,0.6));
#11681=CARTESIAN_POINT('Origin',(-9.6,0.08,0.6));
#11682=CARTESIAN_POINT('',(-9.54222222222222,0.,0.6));
#11683=CARTESIAN_POINT('',(-9.54222222222222,0.,-0.3));
#11684=CARTESIAN_POINT('',(-9.54222222222222,0.,0.3));
#11685=CARTESIAN_POINT('',(-9.6,0.08,0.6));
#11686=CARTESIAN_POINT('',(-7.9355780933063,-2.22458417849898,0.6));
#11687=CARTESIAN_POINT('',(-9.6,0.08,-0.3));
#11688=CARTESIAN_POINT('',(-9.6,0.08,0.6));
#11689=CARTESIAN_POINT('',(-9.09120689655173,-0.624482758620687,-0.3));
#11690=CARTESIAN_POINT('Origin',(-9.665,-0.01,0.6));
#11691=CARTESIAN_POINT('',(-9.65777777777778,0.,-0.3));
#11692=CARTESIAN_POINT('',(-9.65777777777778,0.,0.6));
#11693=CARTESIAN_POINT('',(-9.65777777777778,-2.77555756156289E-17,0.3));
#11694=CARTESIAN_POINT('',(-8.9243559837728,1.01550709939148,-0.3));
#11695=CARTESIAN_POINT('',(-8.00604969574032,2.28700811359028,0.6));
#11696=CARTESIAN_POINT('Origin',(-10.,0.08,0.6));
#11697=CARTESIAN_POINT('',(-9.94222222222222,0.,0.6));
#11698=CARTESIAN_POINT('',(-9.94222222222222,0.,-0.3));
#11699=CARTESIAN_POINT('',(-9.94222222222222,0.,0.3));
#11700=CARTESIAN_POINT('',(-10.,0.08,0.6));
#11701=CARTESIAN_POINT('',(-8.26701825557805,-2.31951318458419,0.6));
#11702=CARTESIAN_POINT('',(-10.,0.08,-0.3));
#11703=CARTESIAN_POINT('',(-10.,0.08,0.6));
#11704=CARTESIAN_POINT('',(-9.42264705882351,-0.71941176470589,-0.3));
#11705=CARTESIAN_POINT('Origin',(-10.065,-0.01,0.6));
#11706=CARTESIAN_POINT('',(-10.0577777777778,0.,-0.3));
#11707=CARTESIAN_POINT('',(-10.0577777777778,0.,0.6));
#11708=CARTESIAN_POINT('',(-10.0577777777778,0.,0.3));
#11709=CARTESIAN_POINT('',(-9.25579614604461,1.11043610547668,-0.3));
#11710=CARTESIAN_POINT('',(-8.33748985801213,2.38193711967547,0.6));
#11711=CARTESIAN_POINT('Origin',(-9.8,0.08,0.6));
#11712=CARTESIAN_POINT('',(-9.74222222222222,0.,0.6));
#11713=CARTESIAN_POINT('',(-9.74222222222222,0.,-0.3));
#11714=CARTESIAN_POINT('',(-9.74222222222222,2.77555756156289E-17,0.3));
#11715=CARTESIAN_POINT('',(-9.8,0.08,0.6));
#11716=CARTESIAN_POINT('',(-8.10129817444215,-2.2720486815416,0.6));
#11717=CARTESIAN_POINT('',(-9.8,0.08,-0.3));
#11718=CARTESIAN_POINT('',(-9.8,0.08,0.6));
#11719=CARTESIAN_POINT('',(-9.25692697768761,-0.671947261663294,-0.3));
#11720=CARTESIAN_POINT('Origin',(-9.865,-0.01,0.6));
#11721=CARTESIAN_POINT('',(-9.85777777777778,0.,-0.3));
#11722=CARTESIAN_POINT('',(-9.85777777777778,0.,0.6));
#11723=CARTESIAN_POINT('',(-9.85777777777778,-2.77555756156289E-17,0.3));
#11724=CARTESIAN_POINT('',(-9.09007606490873,1.06297160243408,-0.3));
#11725=CARTESIAN_POINT('',(-8.17176977687629,2.33447261663285,0.6));
#11726=CARTESIAN_POINT('Origin',(-9.4,0.08,0.6));
#11727=CARTESIAN_POINT('',(-9.34222222222222,0.,0.6));
#11728=CARTESIAN_POINT('',(-9.34222222222222,0.,-0.3));
#11729=CARTESIAN_POINT('',(-9.34222222222222,0.,0.3));
#11730=CARTESIAN_POINT('',(-9.4,0.08,0.6));
#11731=CARTESIAN_POINT('',(-7.76985801217034,-2.1771196754564,0.6));
#11732=CARTESIAN_POINT('',(-9.4,0.08,-0.3));
#11733=CARTESIAN_POINT('',(-9.4,0.08,0.6));
#11734=CARTESIAN_POINT('',(-8.92548681541581,-0.5770182555781,-0.3));
#11735=CARTESIAN_POINT('Origin',(-9.465,-0.01,0.6));
#11736=CARTESIAN_POINT('',(-9.45777777777778,0.,-0.3));
#11737=CARTESIAN_POINT('',(-9.45777777777778,0.,0.6));
#11738=CARTESIAN_POINT('',(-9.45777777777778,0.,0.3));
#11739=CARTESIAN_POINT('',(-8.75863590263692,0.968042596348883,-0.3));
#11740=CARTESIAN_POINT('',(-7.84032961460448,2.23954361054766,0.6));
#11741=CARTESIAN_POINT('Origin',(-9.,0.08,0.6));
#11742=CARTESIAN_POINT('',(-8.94222222222222,0.,0.6));
#11743=CARTESIAN_POINT('',(-8.94222222222222,0.,-0.3));
#11744=CARTESIAN_POINT('',(-8.94222222222222,0.,0.3));
#11745=CARTESIAN_POINT('',(-9.,0.08,0.6));
#11746=CARTESIAN_POINT('',(-7.43841784989854,-2.08219066937121,0.6));
#11747=CARTESIAN_POINT('',(-9.,0.08,-0.3));
#11748=CARTESIAN_POINT('',(-9.,0.08,0.6));
#11749=CARTESIAN_POINT('',(-8.59404665314401,-0.482089249492907,-0.3));
#11750=CARTESIAN_POINT('Origin',(-9.065,-0.01,0.6));
#11751=CARTESIAN_POINT('',(-9.05777777777778,0.,-0.3));
#11752=CARTESIAN_POINT('',(-9.05777777777778,0.,0.6));
#11753=CARTESIAN_POINT('',(-9.05777777777778,0.,0.3));
#11754=CARTESIAN_POINT('',(-8.4271957403651,0.873113590263694,-0.3));
#11755=CARTESIAN_POINT('',(-7.50888945233262,2.14461460446249,0.6));
#11756=CARTESIAN_POINT('Origin',(-8.6,0.08,0.6));
#11757=CARTESIAN_POINT('',(-8.54222222222222,0.,0.6));
#11758=CARTESIAN_POINT('',(-8.54222222222222,0.,-0.3));
#11759=CARTESIAN_POINT('',(-8.54222222222222,0.,0.3));
#11760=CARTESIAN_POINT('',(-8.6,0.08,0.6));
#11761=CARTESIAN_POINT('',(-7.10697768762679,-1.987261663286,0.6));
#11762=CARTESIAN_POINT('',(-8.6,0.08,-0.3));
#11763=CARTESIAN_POINT('',(-8.6,0.08,0.6));
#11764=CARTESIAN_POINT('',(-8.26260649087221,-0.387160243407706,-0.3));
#11765=CARTESIAN_POINT('Origin',(-8.665,-0.01,0.6));
#11766=CARTESIAN_POINT('',(-8.65777777777778,0.,-0.3));
#11767=CARTESIAN_POINT('',(-8.65777777777778,0.,0.6));
#11768=CARTESIAN_POINT('',(-8.65777777777778,0.,0.3));
#11769=CARTESIAN_POINT('',(-8.09575557809329,0.778184584178501,-0.3));
#11770=CARTESIAN_POINT('',(-7.17744929006081,2.0496855983773,0.6));
#11771=CARTESIAN_POINT('Origin',(-8.2,0.08,0.6));
#11772=CARTESIAN_POINT('',(-8.14222222222222,0.,0.6));
#11773=CARTESIAN_POINT('',(-8.14222222222222,0.,-0.3));
#11774=CARTESIAN_POINT('',(-8.14222222222222,1.11022302462516E-16,0.3));
#11775=CARTESIAN_POINT('',(-8.2,0.08,0.6));
#11776=CARTESIAN_POINT('',(-6.77553752535498,-1.89233265720081,0.6));
#11777=CARTESIAN_POINT('',(-8.2,0.08,-0.3));
#11778=CARTESIAN_POINT('',(-8.2,0.08,0.6));
#11779=CARTESIAN_POINT('',(-7.93116632860041,-0.292231237322513,-0.3));
#11780=CARTESIAN_POINT('Origin',(-8.265,-0.01,0.6));
#11781=CARTESIAN_POINT('',(-8.25777777777778,0.,-0.3));
#11782=CARTESIAN_POINT('',(-8.25777777777778,0.,0.6));
#11783=CARTESIAN_POINT('',(-8.25777777777778,0.,0.3));
#11784=CARTESIAN_POINT('',(-7.76431541582149,0.683255578093308,-0.3));
#11785=CARTESIAN_POINT('',(-6.84600912778901,1.9547565922921,0.6));
#11786=CARTESIAN_POINT('Origin',(-7.8,0.08,0.6));
#11787=CARTESIAN_POINT('',(-7.74222222222222,0.,0.6));
#11788=CARTESIAN_POINT('',(-7.74222222222222,0.,-0.3));
#11789=CARTESIAN_POINT('',(-7.74222222222222,0.,0.3));
#11790=CARTESIAN_POINT('',(-7.8,0.08,0.6));
#11791=CARTESIAN_POINT('',(-6.44409736308315,-1.79740365111562,0.6));
#11792=CARTESIAN_POINT('',(-7.8,0.08,-0.3));
#11793=CARTESIAN_POINT('',(-7.8,0.08,0.6));
#11794=CARTESIAN_POINT('',(-7.5997261663286,-0.197302231237324,-0.3));
#11795=CARTESIAN_POINT('Origin',(-7.865,-0.01,0.6));
#11796=CARTESIAN_POINT('',(-7.85777777777778,0.,-0.3));
#11797=CARTESIAN_POINT('',(-7.85777777777778,0.,0.6));
#11798=CARTESIAN_POINT('',(-7.85777777777778,0.,0.3));
#11799=CARTESIAN_POINT('',(-7.43287525354969,0.588326572008114,-0.3));
#11800=CARTESIAN_POINT('',(-6.51456896551723,1.8598275862069,0.6));
#11801=CARTESIAN_POINT('Origin',(-7.4,0.08,0.6));
#11802=CARTESIAN_POINT('',(-7.34222222222222,0.,0.6));
#11803=CARTESIAN_POINT('',(-7.34222222222222,0.,-0.3));
#11804=CARTESIAN_POINT('',(-7.34222222222222,0.,0.3));
#11805=CARTESIAN_POINT('',(-7.4,0.08,0.6));
#11806=CARTESIAN_POINT('',(-6.11265720081133,-1.70247464503044,0.6));
#11807=CARTESIAN_POINT('',(-7.4,0.08,-0.3));
#11808=CARTESIAN_POINT('',(-7.4,0.08,0.6));
#11809=CARTESIAN_POINT('',(-7.26828600405679,-0.102373225152134,-0.3));
#11810=CARTESIAN_POINT('Origin',(-7.465,-0.01,0.6));
#11811=CARTESIAN_POINT('',(-7.45777777777778,0.,-0.3));
#11812=CARTESIAN_POINT('',(-7.45777777777778,0.,0.6));
#11813=CARTESIAN_POINT('',(-7.45777777777778,-1.11022302462516E-16,0.3));
#11814=CARTESIAN_POINT('',(-7.10143509127789,0.493397565922921,-0.3));
#11815=CARTESIAN_POINT('',(-6.18312880324543,1.76489858012171,0.6));
#11816=CARTESIAN_POINT('Origin',(-7.,0.08,0.6));
#11817=CARTESIAN_POINT('',(-6.94222222222222,0.,0.6));
#11818=CARTESIAN_POINT('',(-6.94222222222222,0.,-0.3));
#11819=CARTESIAN_POINT('',(-6.94222222222222,0.,0.3));
#11820=CARTESIAN_POINT('',(-7.,0.08,0.6));
#11821=CARTESIAN_POINT('',(-5.78121703853954,-1.60754563894524,0.6));
#11822=CARTESIAN_POINT('',(-7.,0.08,-0.3));
#11823=CARTESIAN_POINT('',(-7.,0.08,0.6));
#11824=CARTESIAN_POINT('',(-6.93684584178499,-0.00744421906693815,-0.3));
#11825=CARTESIAN_POINT('Origin',(-7.065,-0.01,0.6));
#11826=CARTESIAN_POINT('',(-7.05777777777778,0.,-0.3));
#11827=CARTESIAN_POINT('',(-7.05777777777778,0.,0.6));
#11828=CARTESIAN_POINT('',(-7.05777777777778,-1.11022302462516E-16,0.3));
#11829=CARTESIAN_POINT('',(-6.76999492900608,0.398468559837728,-0.3));
#11830=CARTESIAN_POINT('',(-5.85168864097362,1.66996957403651,0.6));
#11831=CARTESIAN_POINT('Origin',(-6.6,0.08,0.6));
#11832=CARTESIAN_POINT('',(-6.54222222222222,0.,0.6));
#11833=CARTESIAN_POINT('',(-6.54222222222222,0.,-0.3));
#11834=CARTESIAN_POINT('',(-6.54222222222222,0.,0.3));
#11835=CARTESIAN_POINT('',(-6.6,0.08,0.6));
#11836=CARTESIAN_POINT('',(-5.44977687626774,-1.51261663286004,0.6));
#11837=CARTESIAN_POINT('',(-6.6,0.08,-0.3));
#11838=CARTESIAN_POINT('',(-6.6,0.08,0.6));
#11839=CARTESIAN_POINT('',(-6.60540567951318,0.0874847870182548,-0.3));
#11840=CARTESIAN_POINT('Origin',(-6.665,-0.01,0.6));
#11841=CARTESIAN_POINT('',(-6.65777777777778,0.,-0.3));
#11842=CARTESIAN_POINT('',(-6.65777777777778,0.,0.6));
#11843=CARTESIAN_POINT('',(-6.65777777777778,-1.11022302462516E-16,0.3));
#11844=CARTESIAN_POINT('',(-6.43855476673428,0.303539553752534,-0.3));
#11845=CARTESIAN_POINT('',(-5.5202484787018,1.57504056795133,0.6));
#11846=CARTESIAN_POINT('Origin',(-6.4,0.08,0.6));
#11847=CARTESIAN_POINT('',(-6.34222222222222,0.,0.6));
#11848=CARTESIAN_POINT('',(-6.34222222222222,0.,-0.3));
#11849=CARTESIAN_POINT('',(-6.34222222222222,0.,0.3));
#11850=CARTESIAN_POINT('',(-6.4,0.08,0.6));
#11851=CARTESIAN_POINT('',(-5.28405679513184,-1.46515212981745,0.6));
#11852=CARTESIAN_POINT('',(-6.4,0.08,-0.3));
#11853=CARTESIAN_POINT('',(-6.4,0.08,0.6));
#11854=CARTESIAN_POINT('',(-6.43968559837728,0.134949290060851,-0.3));
#11855=CARTESIAN_POINT('Origin',(-6.465,-0.01,0.6));
#11856=CARTESIAN_POINT('',(-6.45777777777778,0.,-0.3));
#11857=CARTESIAN_POINT('',(-6.45777777777778,0.,0.6));
#11858=CARTESIAN_POINT('',(-6.45777777777778,1.11022302462516E-16,0.3));
#11859=CARTESIAN_POINT('',(-6.27283468559838,0.256075050709939,-0.3));
#11860=CARTESIAN_POINT('',(-5.35452839756591,1.52757606490873,0.6));
#11861=CARTESIAN_POINT('Origin',(-6.,0.08,0.6));
#11862=CARTESIAN_POINT('',(-5.94222222222222,0.,0.6));
#11863=CARTESIAN_POINT('',(-5.94222222222222,0.,-0.3));
#11864=CARTESIAN_POINT('',(-5.94222222222222,2.22044604925031E-16,0.3));
#11865=CARTESIAN_POINT('',(-6.,0.08,0.6));
#11866=CARTESIAN_POINT('',(-4.95261663286005,-1.37022312373225,0.6));
#11867=CARTESIAN_POINT('',(-6.,0.08,-0.3));
#11868=CARTESIAN_POINT('',(-6.,0.08,0.6));
#11869=CARTESIAN_POINT('',(-6.10824543610548,0.229878296146045,-0.3));
#11870=CARTESIAN_POINT('Origin',(-6.065,-0.01,0.6));
#11871=CARTESIAN_POINT('',(-6.05777777777778,0.,-0.3));
#11872=CARTESIAN_POINT('',(-6.05777777777778,0.,0.6));
#11873=CARTESIAN_POINT('',(-6.05777777777778,0.,0.3));
#11874=CARTESIAN_POINT('',(-5.94139452332657,0.161146044624747,-0.3));
#11875=CARTESIAN_POINT('',(-5.02308823529413,1.43264705882353,0.6));
#11876=CARTESIAN_POINT('Origin',(-5.6,0.08,0.6));
#11877=CARTESIAN_POINT('',(-5.54222222222222,0.,0.6));
#11878=CARTESIAN_POINT('',(-5.54222222222222,0.,-0.3));
#11879=CARTESIAN_POINT('',(-5.54222222222222,0.,0.3));
#11880=CARTESIAN_POINT('',(-5.6,0.08,0.6));
#11881=CARTESIAN_POINT('',(-4.62117647058824,-1.27529411764706,0.6));
#11882=CARTESIAN_POINT('',(-5.6,0.08,-0.3));
#11883=CARTESIAN_POINT('',(-5.6,0.08,0.6));
#11884=CARTESIAN_POINT('',(-5.77680527383367,0.324807302231238,-0.3));
#11885=CARTESIAN_POINT('Origin',(-5.665,-0.01,0.6));
#11886=CARTESIAN_POINT('',(-5.65777777777778,0.,-0.3));
#11887=CARTESIAN_POINT('',(-5.65777777777778,0.,0.6));
#11888=CARTESIAN_POINT('',(-5.65777777777778,0.,0.3));
#11889=CARTESIAN_POINT('',(-5.60995436105477,0.066217038539553,-0.3));
#11890=CARTESIAN_POINT('',(-4.6916480730223,1.33771805273834,0.6));
#11891=CARTESIAN_POINT('Origin',(-5.2,0.08,0.6));
#11892=CARTESIAN_POINT('',(-5.14222222222222,0.,0.6));
#11893=CARTESIAN_POINT('',(-5.14222222222222,0.,-0.3));
#11894=CARTESIAN_POINT('',(-5.14222222222222,2.22044604925031E-16,0.3));
#11895=CARTESIAN_POINT('',(-5.2,0.08,0.6));
#11896=CARTESIAN_POINT('',(-4.28973630831642,-1.18036511156187,0.6));
#11897=CARTESIAN_POINT('',(-5.2,0.08,-0.3));
#11898=CARTESIAN_POINT('',(-5.2,0.08,0.6));
#11899=CARTESIAN_POINT('',(-5.44536511156187,0.41973630831643,-0.3));
#11900=CARTESIAN_POINT('Origin',(-5.265,-0.01,0.6));
#11901=CARTESIAN_POINT('',(-5.25777777777778,0.,-0.3));
#11902=CARTESIAN_POINT('',(-5.25777777777778,0.,0.6));
#11903=CARTESIAN_POINT('',(-5.25777777777778,0.,0.3));
#11904=CARTESIAN_POINT('',(-5.27851419878296,-0.0287119675456377,-0.3));
#11905=CARTESIAN_POINT('',(-4.36020791075052,1.24278904665314,0.6));
#11906=CARTESIAN_POINT('Origin',(-4.8,0.08,0.6));
#11907=CARTESIAN_POINT('',(-4.74222222222222,0.,0.6));
#11908=CARTESIAN_POINT('',(-4.74222222222222,0.,-0.3));
#11909=CARTESIAN_POINT('',(-4.74222222222222,2.22044604925031E-16,0.3));
#11910=CARTESIAN_POINT('',(-4.8,0.08,0.6));
#11911=CARTESIAN_POINT('',(-3.95829614604463,-1.08543610547667,0.6));
#11912=CARTESIAN_POINT('',(-4.8,0.08,-0.3));
#11913=CARTESIAN_POINT('',(-4.8,0.08,0.6));
#11914=CARTESIAN_POINT('',(-5.11392494929006,0.514665314401623,-0.3));
#11915=CARTESIAN_POINT('Origin',(-4.865,-0.01,0.6));
#11916=CARTESIAN_POINT('',(-4.85777777777778,0.,-0.3));
#11917=CARTESIAN_POINT('',(-4.85777777777778,0.,0.6));
#11918=CARTESIAN_POINT('',(-4.85777777777778,-2.22044604925031E-16,0.3));
#11919=CARTESIAN_POINT('',(-4.94707403651116,-0.123640973630833,-0.3));
#11920=CARTESIAN_POINT('',(-4.0287677484787,1.14786004056795,0.6));
#11921=CARTESIAN_POINT('Origin',(-4.4,0.08,0.6));
#11922=CARTESIAN_POINT('',(-4.34222222222222,0.,0.6));
#11923=CARTESIAN_POINT('',(-4.34222222222222,0.,-0.3));
#11924=CARTESIAN_POINT('',(-4.34222222222222,0.,0.3));
#11925=CARTESIAN_POINT('',(-4.4,0.08,0.6));
#11926=CARTESIAN_POINT('',(-3.62685598377281,-0.990507099391483,0.6));
#11927=CARTESIAN_POINT('',(-4.4,0.08,-0.3));
#11928=CARTESIAN_POINT('',(-4.4,0.08,0.6));
#11929=CARTESIAN_POINT('',(-4.78248478701826,0.609594320486815,-0.3));
#11930=CARTESIAN_POINT('Origin',(-4.465,-0.01,0.6));
#11931=CARTESIAN_POINT('',(-4.45777777777778,0.,-0.3));
#11932=CARTESIAN_POINT('',(-4.45777777777778,0.,0.6));
#11933=CARTESIAN_POINT('',(-4.45777777777778,0.,0.3));
#11934=CARTESIAN_POINT('',(-4.61563387423935,-0.218569979716023,-0.3));
#11935=CARTESIAN_POINT('',(-3.6973275862069,1.05293103448276,0.6));
#11936=CARTESIAN_POINT('Origin',(-4.,0.08,0.6));
#11937=CARTESIAN_POINT('',(-3.94222222222222,0.,0.6));
#11938=CARTESIAN_POINT('',(-3.94222222222222,0.,-0.3));
#11939=CARTESIAN_POINT('',(-3.94222222222222,0.,0.3));
#11940=CARTESIAN_POINT('',(-4.,0.08,0.6));
#11941=CARTESIAN_POINT('',(-3.29541582150101,-0.895578093306288,0.6));
#11942=CARTESIAN_POINT('',(-4.,0.08,-0.3));
#11943=CARTESIAN_POINT('',(-4.,0.08,0.6));
#11944=CARTESIAN_POINT('',(-4.45104462474645,0.704523326572008,-0.3));
#11945=CARTESIAN_POINT('Origin',(-4.065,-0.01,0.6));
#11946=CARTESIAN_POINT('',(-4.05777777777778,0.,-0.3));
#11947=CARTESIAN_POINT('',(-4.05777777777778,0.,0.6));
#11948=CARTESIAN_POINT('',(-4.05777777777778,-2.22044604925031E-16,0.3));
#11949=CARTESIAN_POINT('',(-4.28419371196754,-0.313498985801215,-0.3));
#11950=CARTESIAN_POINT('',(-3.3658874239351,0.958002028397564,0.6));
#11951=CARTESIAN_POINT('Origin',(-3.6,0.08,0.6));
#11952=CARTESIAN_POINT('',(-3.54222222222222,0.,0.6));
#11953=CARTESIAN_POINT('',(-3.54222222222222,0.,-0.3));
#11954=CARTESIAN_POINT('',(-3.54222222222222,-2.22044604925031E-16,0.3));
#11955=CARTESIAN_POINT('',(-3.6,0.08,0.6));
#11956=CARTESIAN_POINT('',(-2.96397565922921,-0.800649087221095,0.6));
#11957=CARTESIAN_POINT('',(-3.6,0.08,-0.3));
#11958=CARTESIAN_POINT('',(-3.6,0.08,0.6));
#11959=CARTESIAN_POINT('',(-4.11960446247465,0.799452332657201,-0.3));
#11960=CARTESIAN_POINT('Origin',(-3.665,-0.01,0.6));
#11961=CARTESIAN_POINT('',(-3.65777777777778,0.,-0.3));
#11962=CARTESIAN_POINT('',(-3.65777777777778,0.,0.6));
#11963=CARTESIAN_POINT('',(-3.65777777777778,2.22044604925031E-16,0.3));
#11964=CARTESIAN_POINT('',(-3.95275354969574,-0.40842799188641,-0.3));
#11965=CARTESIAN_POINT('',(-3.03444726166329,0.863073022312373,0.6));
#11966=CARTESIAN_POINT('Origin',(-3.2,0.08,0.6));
#11967=CARTESIAN_POINT('',(-3.14222222222222,0.,0.6));
#11968=CARTESIAN_POINT('',(-3.14222222222222,0.,-0.3));
#11969=CARTESIAN_POINT('',(-3.14222222222222,-2.22044604925031E-16,0.3));
#11970=CARTESIAN_POINT('',(-3.2,0.08,0.6));
#11971=CARTESIAN_POINT('',(-2.6325354969574,-0.705720081135902,0.6));
#11972=CARTESIAN_POINT('',(-3.2,0.08,-0.3));
#11973=CARTESIAN_POINT('',(-3.2,0.08,0.6));
#11974=CARTESIAN_POINT('',(-3.78816430020284,0.894381338742393,-0.3));
#11975=CARTESIAN_POINT('Origin',(-3.265,-0.01,0.6));
#11976=CARTESIAN_POINT('',(-3.25777777777778,0.,-0.3));
#11977=CARTESIAN_POINT('',(-3.25777777777778,0.,0.6));
#11978=CARTESIAN_POINT('',(-3.25777777777778,-2.22044604925031E-16,0.3));
#11979=CARTESIAN_POINT('',(-3.62131338742393,-0.5033569979716,-0.3));
#11980=CARTESIAN_POINT('',(-2.70300709939149,0.768144016227179,0.6));
#11981=CARTESIAN_POINT('Origin',(-2.8,0.08,0.6));
#11982=CARTESIAN_POINT('',(-2.74222222222222,0.,0.6));
#11983=CARTESIAN_POINT('',(-2.74222222222222,0.,-0.3));
#11984=CARTESIAN_POINT('',(-2.74222222222222,0.,0.3));
#11985=CARTESIAN_POINT('',(-2.8,0.08,0.6));
#11986=CARTESIAN_POINT('',(-2.3010953346856,-0.610791075050709,0.6));
#11987=CARTESIAN_POINT('',(-2.8,0.08,-0.3));
#11988=CARTESIAN_POINT('',(-2.8,0.08,0.6));
#11989=CARTESIAN_POINT('',(-3.45672413793103,0.989310344827585,-0.3));
#11990=CARTESIAN_POINT('Origin',(-2.865,-0.01,0.6));
#11991=CARTESIAN_POINT('',(-2.85777777777778,0.,-0.3));
#11992=CARTESIAN_POINT('',(-2.85777777777778,0.,0.6));
#11993=CARTESIAN_POINT('',(-2.85777777777778,0.,0.3));
#11994=CARTESIAN_POINT('',(-3.28987322515213,-0.598286004056795,-0.3));
#11995=CARTESIAN_POINT('',(-2.37156693711968,0.673215010141988,0.6));
#11996=CARTESIAN_POINT('Origin',(-10.5,0.,0.));
#11997=CARTESIAN_POINT('',(-1.6,0.,-0.3));
#11998=CARTESIAN_POINT('',(-1.6,0.,-0.3));
#11999=CARTESIAN_POINT('',(-1.6,0.,0.));
#12000=CARTESIAN_POINT('',(-1.6,0.,-0.3));
#12001=CARTESIAN_POINT('',(-1.4,0.,0.));
#12002=CARTESIAN_POINT('',(-1.2,0.,0.));
#12003=CARTESIAN_POINT('',(-1.4,0.,0.6));
#12004=CARTESIAN_POINT('',(-1.4,0.,0.));
#12005=CARTESIAN_POINT('',(-1.2,0.,0.6));
#12006=CARTESIAN_POINT('Origin',(-10.5,0.,0.));
#12007=CARTESIAN_POINT('',(-1.6,0.,-0.3));
#12008=CARTESIAN_POINT('',(-1.2,0.,0.6));
#12009=CARTESIAN_POINT('Origin',(-10.5,0.,0.));
#12010=CARTESIAN_POINT('',(-1.6,0.,-0.3));
#12011=CARTESIAN_POINT('',(-1.2,0.,0.6));
#12012=CARTESIAN_POINT('Origin',(-10.5,0.,0.));
#12013=CARTESIAN_POINT('',(-1.6,0.,-0.3));
#12014=CARTESIAN_POINT('',(-1.2,0.,0.6));
#12015=CARTESIAN_POINT('Origin',(-10.5,0.,0.));
#12016=CARTESIAN_POINT('',(-1.6,0.,-0.3));
#12017=CARTESIAN_POINT('',(-1.2,0.,0.6));
#12018=CARTESIAN_POINT('Origin',(-10.5,0.,0.));
#12019=CARTESIAN_POINT('',(-1.6,0.,-0.3));
#12020=CARTESIAN_POINT('',(-1.2,0.,0.6));
#12021=CARTESIAN_POINT('Origin',(-10.5,0.,0.));
#12022=CARTESIAN_POINT('',(-1.6,0.,-0.3));
#12023=CARTESIAN_POINT('',(-1.2,0.,0.6));
#12024=CARTESIAN_POINT('Origin',(-10.5,0.,0.));
#12025=CARTESIAN_POINT('',(-1.6,0.,-0.3));
#12026=CARTESIAN_POINT('',(-1.2,0.,0.6));
#12027=CARTESIAN_POINT('Origin',(-10.5,0.,0.));
#12028=CARTESIAN_POINT('',(-1.6,0.,-0.3));
#12029=CARTESIAN_POINT('',(-1.2,0.,0.6));
#12030=CARTESIAN_POINT('Origin',(-10.5,0.,0.));
#12031=CARTESIAN_POINT('',(-1.6,0.,-0.3));
#12032=CARTESIAN_POINT('',(-1.2,0.,0.6));
#12033=CARTESIAN_POINT('Origin',(-10.5,0.,0.));
#12034=CARTESIAN_POINT('',(-1.6,0.,-0.3));
#12035=CARTESIAN_POINT('',(-1.2,0.,0.6));
#12036=CARTESIAN_POINT('Origin',(-10.5,0.,0.));
#12037=CARTESIAN_POINT('',(-1.6,0.,-0.3));
#12038=CARTESIAN_POINT('',(-1.2,0.,0.6));
#12039=CARTESIAN_POINT('Origin',(-10.5,0.,0.));
#12040=CARTESIAN_POINT('',(-1.6,0.,-0.3));
#12041=CARTESIAN_POINT('',(-1.2,0.,0.6));
#12042=CARTESIAN_POINT('Origin',(-10.5,0.,0.));
#12043=CARTESIAN_POINT('',(-1.6,0.,-0.3));
#12044=CARTESIAN_POINT('',(-1.2,0.,0.6));
#12045=CARTESIAN_POINT('Origin',(-10.5,0.,0.));
#12046=CARTESIAN_POINT('',(-1.6,0.,-0.3));
#12047=CARTESIAN_POINT('',(-1.2,0.,0.6));
#12048=CARTESIAN_POINT('Origin',(-10.5,0.,0.));
#12049=CARTESIAN_POINT('',(-1.6,0.,-0.3));
#12050=CARTESIAN_POINT('',(-1.2,0.,0.6));
#12051=CARTESIAN_POINT('Origin',(-10.5,0.,0.));
#12052=CARTESIAN_POINT('',(-1.6,0.,-0.3));
#12053=CARTESIAN_POINT('',(-1.2,0.,0.6));
#12054=CARTESIAN_POINT('Origin',(-10.5,0.,0.));
#12055=CARTESIAN_POINT('',(-1.6,0.,-0.3));
#12056=CARTESIAN_POINT('',(-1.2,0.,0.6));
#12057=CARTESIAN_POINT('Origin',(-10.5,0.,0.));
#12058=CARTESIAN_POINT('',(-1.6,0.,-0.3));
#12059=CARTESIAN_POINT('',(-1.2,0.,0.6));
#12060=CARTESIAN_POINT('Origin',(-10.5,0.,0.));
#12061=CARTESIAN_POINT('',(-1.6,0.,-0.3));
#12062=CARTESIAN_POINT('',(-1.2,0.,0.6));
#12063=CARTESIAN_POINT('Origin',(-10.5,0.,0.));
#12064=CARTESIAN_POINT('',(-1.6,0.,-0.3));
#12065=CARTESIAN_POINT('',(-1.2,0.,0.6));
#12066=CARTESIAN_POINT('Origin',(-10.5,0.,0.));
#12067=CARTESIAN_POINT('',(-1.2,0.,0.6));
#12068=CARTESIAN_POINT('',(-1.6,0.,-0.3));
#12069=CARTESIAN_POINT('Origin',(-10.5,0.,0.));
#12070=CARTESIAN_POINT('',(-1.2,0.,0.6));
#12071=CARTESIAN_POINT('',(-1.6,0.,-0.3));
#12072=CARTESIAN_POINT('Origin',(-10.5,0.,0.));
#12073=CARTESIAN_POINT('',(-1.2,0.,0.6));
#12074=CARTESIAN_POINT('',(-1.6,0.,-0.3));
#12075=CARTESIAN_POINT('Origin',(-10.5,0.,0.));
#12076=CARTESIAN_POINT('',(-1.2,0.,0.6));
#12077=CARTESIAN_POINT('',(-1.6,0.,-0.3));
#12078=CARTESIAN_POINT('Origin',(-10.5,0.,0.));
#12079=CARTESIAN_POINT('',(-1.2,0.,0.6));
#12080=CARTESIAN_POINT('',(-1.6,0.,-0.3));
#12081=CARTESIAN_POINT('Origin',(-10.5,0.,0.));
#12082=CARTESIAN_POINT('',(-1.2,0.,0.6));
#12083=CARTESIAN_POINT('',(-1.6,0.,-0.3));
#12084=CARTESIAN_POINT('Origin',(-10.5,0.,0.));
#12085=CARTESIAN_POINT('',(-1.2,0.,0.6));
#12086=CARTESIAN_POINT('',(-1.6,0.,-0.3));
#12087=CARTESIAN_POINT('Origin',(-10.5,0.,0.));
#12088=CARTESIAN_POINT('',(-1.2,0.,0.6));
#12089=CARTESIAN_POINT('',(-1.6,0.,-0.3));
#12090=CARTESIAN_POINT('Origin',(-10.5,0.,0.));
#12091=CARTESIAN_POINT('',(-10.5,0.,0.6));
#12092=CARTESIAN_POINT('',(-1.2,0.,0.6));
#12093=CARTESIAN_POINT('',(-10.5,0.,-0.3));
#12094=CARTESIAN_POINT('',(-10.5,0.,0.));
#12095=CARTESIAN_POINT('',(-1.6,0.,-0.3));
#12096=CARTESIAN_POINT('Origin',(-10.5,0.,0.));
#12097=CARTESIAN_POINT('',(-1.2,0.,0.6));
#12098=CARTESIAN_POINT('',(-1.6,0.,-0.3));
#12099=CARTESIAN_POINT('Origin',(-10.5,0.,0.));
#12100=CARTESIAN_POINT('',(-1.2,0.,0.6));
#12101=CARTESIAN_POINT('',(-1.6,0.,-0.3));
#12102=CARTESIAN_POINT('Origin',(-10.5,0.,0.));
#12103=CARTESIAN_POINT('',(-1.2,0.,0.6));
#12104=CARTESIAN_POINT('',(-1.6,0.,-0.3));
#12105=CARTESIAN_POINT('Origin',(-10.5,0.,0.));
#12106=CARTESIAN_POINT('',(-1.2,0.,0.6));
#12107=CARTESIAN_POINT('',(-1.6,0.,-0.3));
#12108=CARTESIAN_POINT('Origin',(-10.5,0.,0.));
#12109=CARTESIAN_POINT('',(-1.2,0.,0.6));
#12110=CARTESIAN_POINT('',(-1.6,0.,-0.3));
#12111=CARTESIAN_POINT('Origin',(-10.5,0.,0.));
#12112=CARTESIAN_POINT('',(-1.2,0.,0.6));
#12113=CARTESIAN_POINT('',(-1.6,0.,-0.3));
#12114=CARTESIAN_POINT('Origin',(-10.5,0.,0.));
#12115=CARTESIAN_POINT('',(-1.2,0.,0.6));
#12116=CARTESIAN_POINT('',(-1.6,0.,-0.3));
#12117=CARTESIAN_POINT('Origin',(-10.5,0.,0.));
#12118=CARTESIAN_POINT('',(-1.2,0.,0.6));
#12119=CARTESIAN_POINT('',(-1.6,0.,-0.3));
#12120=CARTESIAN_POINT('Origin',(-10.5,0.,0.));
#12121=CARTESIAN_POINT('',(-1.2,0.,0.6));
#12122=CARTESIAN_POINT('',(-1.6,0.,-0.3));
#12123=CARTESIAN_POINT('Origin',(-6.05,0.5,-0.3));
#12124=CARTESIAN_POINT('',(-10.5,0.2,-0.3));
#12125=CARTESIAN_POINT('',(-10.5,0.,-0.3));
#12126=CARTESIAN_POINT('',(-2.8,1.,-0.3));
#12127=CARTESIAN_POINT('',(-10.5,0.2,-0.3));
#12128=CARTESIAN_POINT('',(-1.6,1.,-0.3));
#12129=CARTESIAN_POINT('',(-2.8,1.,-0.3));
#12130=CARTESIAN_POINT('',(-1.6,1.,-0.3));
#12131=CARTESIAN_POINT('Origin',(-1.6,0.,-0.3));
#12132=CARTESIAN_POINT('',(-1.6,1.,0.));
#12133=CARTESIAN_POINT('',(-1.6,1.,-0.3));
#12134=CARTESIAN_POINT('',(-1.6,0.,0.));
#12135=CARTESIAN_POINT('Origin',(-1.2,0.,0.));
#12136=CARTESIAN_POINT('',(-1.2,0.721110255092798,0.));
#12137=CARTESIAN_POINT('',(-1.2,0.721110255092798,0.6));
#12138=CARTESIAN_POINT('',(-1.2,0.721110255092798,0.));
#12139=CARTESIAN_POINT('',(-1.2,1.,0.));
#12140=CARTESIAN_POINT('',(-1.2,1.,0.));
#12141=CARTESIAN_POINT('',(-1.2,1.,0.6));
#12142=CARTESIAN_POINT('',(-1.2,1.,0.));
#12143=CARTESIAN_POINT('',(-1.2,1.,0.6));
#12144=CARTESIAN_POINT('Origin',(-10.5,0.2,0.));
#12145=CARTESIAN_POINT('',(-10.5,0.2,0.6));
#12146=CARTESIAN_POINT('',(-10.5,0.,0.6));
#12147=CARTESIAN_POINT('',(-10.5,0.2,0.));
#12148=CARTESIAN_POINT('Origin',(-2.8,1.,0.));
#12149=CARTESIAN_POINT('',(-2.8,1.,0.6));
#12150=CARTESIAN_POINT('',(-10.5,0.2,0.6));
#12151=CARTESIAN_POINT('',(-2.8,1.,0.));
#12152=CARTESIAN_POINT('Origin',(-1.2,1.,0.));
#12153=CARTESIAN_POINT('',(-2.8,1.,0.6));
#12154=CARTESIAN_POINT('',(-2.8,1.,0.));
#12155=CARTESIAN_POINT('Origin',(0.,0.,0.));
#12156=CARTESIAN_POINT('',(0.993295878967653,0.986591757935306,0.));
#12157=CARTESIAN_POINT('Origin',(0.,0.,0.));
#12158=CARTESIAN_POINT('',(1.,1.,0.));
#12159=CARTESIAN_POINT('',(1.,1.,0.));
#12160=CARTESIAN_POINT('',(3.8,-1.9,0.));
#12161=CARTESIAN_POINT('',(3.8,-1.9,0.));
#12162=CARTESIAN_POINT('',(14.,-1.9,0.));
#12163=CARTESIAN_POINT('',(14.,-1.9,0.));
#12164=CARTESIAN_POINT('',(14.,-3.1,0.));
#12165=CARTESIAN_POINT('',(14.,-3.1,0.));
#12166=CARTESIAN_POINT('',(3.8,-3.1,0.));
#12167=CARTESIAN_POINT('',(3.8,-3.1,0.));
#12168=CARTESIAN_POINT('',(0.533017816115691,-1.29456247732709,0.));
#12169=CARTESIAN_POINT('',(0.,-1.,0.));
#12170=CARTESIAN_POINT('Origin',(0.,0.,0.));
#12171=CARTESIAN_POINT('Origin',(0.,0.,0.));
#12172=CARTESIAN_POINT('',(0.993295878967653,0.986591757935306,0.6));
#12173=CARTESIAN_POINT('Origin',(0.,0.,0.6));
#12174=CARTESIAN_POINT('',(0.993295878967653,0.986591757935306,0.));
#12175=CARTESIAN_POINT('Origin',(0.,-1.,0.));
#12176=CARTESIAN_POINT('',(0.533017816115691,-1.29456247732709,0.6));
#12177=CARTESIAN_POINT('',(0.533017816115691,-1.29456247732709,0.));
#12178=CARTESIAN_POINT('',(3.8,-3.1,0.6));
#12179=CARTESIAN_POINT('',(3.8,-3.1,0.));
#12180=CARTESIAN_POINT('',(0.,-1.,0.6));
#12181=CARTESIAN_POINT('Origin',(1.,1.,0.));
#12182=CARTESIAN_POINT('',(1.,1.,0.6));
#12183=CARTESIAN_POINT('',(1.,1.,0.6));
#12184=CARTESIAN_POINT('',(1.,1.,0.));
#12185=CARTESIAN_POINT('Origin',(3.8,-1.9,0.));
#12186=CARTESIAN_POINT('',(3.8,-1.9,0.6));
#12187=CARTESIAN_POINT('',(3.8,-1.9,0.6));
#12188=CARTESIAN_POINT('',(3.8,-1.9,0.));
#12189=CARTESIAN_POINT('Origin',(14.,-1.9,0.));
#12190=CARTESIAN_POINT('',(14.,-1.9,0.6));
#12191=CARTESIAN_POINT('',(14.,-1.9,0.6));
#12192=CARTESIAN_POINT('',(14.,-1.9,0.));
#12193=CARTESIAN_POINT('Origin',(14.,-3.1,0.));
#12194=CARTESIAN_POINT('',(14.,-3.1,0.6));
#12195=CARTESIAN_POINT('',(14.,-3.1,0.6));
#12196=CARTESIAN_POINT('',(14.,-3.1,0.));
#12197=CARTESIAN_POINT('Origin',(3.8,-3.1,0.));
#12198=CARTESIAN_POINT('',(3.8,-3.1,0.6));
#12199=CARTESIAN_POINT('Origin',(0.,0.,0.6));
#12200=CARTESIAN_POINT('Origin',(0.,0.,0.6));
#12201=CARTESIAN_POINT('Origin',(0.,0.,0.));
#12202=CARTESIAN_POINT('',(0.,0.,0.));
#12203=CARTESIAN_POINT('Origin',(0.,0.,0.75));
#12204=CARTESIAN_POINT('',(-0.3,-3.67394039744206E-17,0.7));
#12205=CARTESIAN_POINT('Origin',(0.,0.,0.7));
#12206=CARTESIAN_POINT('',(-0.3,-3.67394039744206E-17,0.8));
#12207=CARTESIAN_POINT('',(-0.3,-3.67394039744206E-17,0.75));
#12208=CARTESIAN_POINT('Origin',(0.,0.,0.8));
#12209=CARTESIAN_POINT('Origin',(0.7,0.,0.7));
#12210=CARTESIAN_POINT('',(-0.4,4.89858719658941E-17,0.7));
#12211=CARTESIAN_POINT('Origin',(0.,0.,0.7));
#12212=CARTESIAN_POINT('Origin',(0.3,0.,0.8));
#12213=CARTESIAN_POINT('',(-0.4,-4.89858719658941E-17,0.8));
#12214=CARTESIAN_POINT('Origin',(0.,0.,0.8));
#12215=CARTESIAN_POINT('Origin',(0.,0.,-0.7));
#12216=CARTESIAN_POINT('',(-0.4,-4.89858719658941E-17,0.9));
#12217=CARTESIAN_POINT('Origin',(0.,0.,0.9));
#12218=CARTESIAN_POINT('',(-0.4,-4.89858719658941E-17,-0.7));
#12219=CARTESIAN_POINT('Origin',(0.,0.,-0.7));
#12220=CARTESIAN_POINT('',(-0.6,-7.34788079488412E-17,-0.7));
#12221=CARTESIAN_POINT('Origin',(0.,0.,-0.7));
#12222=CARTESIAN_POINT('',(-0.4,-4.89858719658941E-17,-0.7));
#12223=CARTESIAN_POINT('Origin',(0.,0.,-0.7));
#12224=CARTESIAN_POINT('Origin',(0.,0.,-0.8));
#12225=CARTESIAN_POINT('',(-0.6,-7.34788079488412E-17,-0.8));
#12226=CARTESIAN_POINT('',(-0.6,-7.34788079488412E-17,-0.8));
#12227=CARTESIAN_POINT('Origin',(0.,0.,-0.8));
#12228=CARTESIAN_POINT('Origin',(0.,0.,-0.8));
#12229=CARTESIAN_POINT('Origin',(0.,0.,-0.7));
#12230=CARTESIAN_POINT('',(-0.4,-4.89858719658941E-17,-0.7));
#12231=CARTESIAN_POINT('Origin',(0.,0.,0.9));
#12232=CARTESIAN_POINT('',(0.,0.,0.));
#12233=CARTESIAN_POINT('Origin',(-0.1,0.,0.1));
#12234=CARTESIAN_POINT('',(-0.1,0.282842712474619,0.));
#12235=CARTESIAN_POINT('',(-0.1,0.282842712474619,0.1));
#12236=CARTESIAN_POINT('',(-0.1,0.282842712474619,0.));
#12237=CARTESIAN_POINT('',(-0.1,0.591607978309962,0.));
#12238=CARTESIAN_POINT('',(-0.1,0.,0.));
#12239=CARTESIAN_POINT('',(-0.1,0.591607978309962,0.1));
#12240=CARTESIAN_POINT('',(-0.1,0.591607978309962,0.));
#12241=CARTESIAN_POINT('',(-0.1,0.,0.1));
#12242=CARTESIAN_POINT('Origin',(0.1,1.2,0.1));
#12243=CARTESIAN_POINT('',(0.1,0.282842712474619,0.1));
#12244=CARTESIAN_POINT('',(0.1,0.282842712474619,0.));
#12245=CARTESIAN_POINT('',(0.1,0.282842712474619,0.));
#12246=CARTESIAN_POINT('',(0.1,0.591607978309962,0.1));
#12247=CARTESIAN_POINT('',(0.1,0.6,0.1));
#12248=CARTESIAN_POINT('',(0.1,0.591607978309962,0.));
#12249=CARTESIAN_POINT('',(0.1,0.591607978309962,0.));
#12250=CARTESIAN_POINT('',(0.1,0.6,0.));
#12251=CARTESIAN_POINT('Origin',(0.,0.,0.));
#12252=CARTESIAN_POINT('Origin',(0.,0.,0.));
#12253=CARTESIAN_POINT('Origin',(0.,0.,0.));
#12254=CARTESIAN_POINT('Origin',(0.,0.,0.));
#12255=CARTESIAN_POINT('Origin',(0.,0.,0.1));
#12256=CARTESIAN_POINT('Origin',(0.,0.,0.));
#12257=CARTESIAN_POINT('Origin',(0.,0.,0.1));
#12258=CARTESIAN_POINT('Origin',(0.,0.,0.1));
#12259=CARTESIAN_POINT('',(0.,0.,0.));
#12260=CARTESIAN_POINT('',(0.,0.,0.));
#12261=CARTESIAN_POINT('Origin',(8.1,-1.,0.7));
#12262=CARTESIAN_POINT('',(7.94916965151797,-1.19937453693185,0.7));
#12263=CARTESIAN_POINT('',(8.26514540988519,-1.18768855477586,0.7));
#12264=CARTESIAN_POINT('Ctrl Pts',(7.94916965151797,-1.19937453693185,0.7));
#12265=CARTESIAN_POINT('Ctrl Pts',(7.97160858810976,-1.21634998764782,0.7));
#12266=CARTESIAN_POINT('Ctrl Pts',(7.99739856866269,-1.22989011121344,0.69528529300377));
#12267=CARTESIAN_POINT('Ctrl Pts',(8.03944443766207,-1.24298414277179,0.688517705185315));
#12268=CARTESIAN_POINT('Ctrl Pts',(8.05362924383607,-1.24609346022897,0.686388676887586));
#12269=CARTESIAN_POINT('Ctrl Pts',(8.075506183533,-1.24890990228851,0.684139035126277));
#12270=CARTESIAN_POINT('Ctrl Pts',(8.08297567221474,-1.24953307703463,0.683546226354886));
#12271=CARTESIAN_POINT('Ctrl Pts',(8.0940066533036,-1.24995288972095,0.68299521602547));
#12272=CARTESIAN_POINT('Ctrl Pts',(8.09752287926269,-1.25001251279495,0.68286729538075));
#12273=CARTESIAN_POINT('Ctrl Pts',(8.10293413375911,-1.249989933108,0.682747340264197));
#12274=CARTESIAN_POINT('Ctrl Pts',(8.10482478940148,-1.24996059450444,0.682719828470948));
#12275=CARTESIAN_POINT('Ctrl Pts',(8.10828546792054,-1.24986760009171,0.682696100760705));
#12276=CARTESIAN_POINT('Ctrl Pts',(8.10985478687837,-1.24981062779486,0.682695370268813));
#12277=CARTESIAN_POINT('Ctrl Pts',(8.11326464342549,-1.24965465239671,0.682715595753076));
#12278=CARTESIAN_POINT('Ctrl Pts',(8.11510409202247,-1.2495501177419,0.682740330911594));
#12279=CARTESIAN_POINT('Ctrl Pts',(8.12014207260669,-1.24920790966494,0.682845651127781));
#12280=CARTESIAN_POINT('Ctrl Pts',(8.12333423895876,-1.24892926854386,0.682953992816581));
#12281=CARTESIAN_POINT('Ctrl Pts',(8.139194120874,-1.2472372768871,0.683691668462565));
#12282=CARTESIAN_POINT('Ctrl Pts',(8.15164141295685,-1.2449338270761,0.684918799511701));
#12283=CARTESIAN_POINT('Ctrl Pts',(8.19196937649467,-1.23428099896052,0.690212518998986));
#12284=CARTESIAN_POINT('Ctrl Pts',(8.21811504697062,-1.22213176592155,0.695755006185672));
#12285=CARTESIAN_POINT('Ctrl Pts',(8.24962874265135,-1.20052913769617,0.699397421419897));
#12286=CARTESIAN_POINT('Ctrl Pts',(8.25758631484639,-1.19433973204149,0.7));
#12287=CARTESIAN_POINT('Ctrl Pts',(8.26514540988519,-1.18768855477586,0.7));
#12288=CARTESIAN_POINT('Origin',(8.1,-1.,0.7));
#12289=CARTESIAN_POINT('Origin',(2.7,1.,0.7));
#12290=CARTESIAN_POINT('',(2.8076286513348,1.22564590451442,0.7));
#12291=CARTESIAN_POINT('',(2.57739843082973,1.21787348447435,0.7));
#12292=CARTESIAN_POINT('Ctrl Pts',(2.80762864495888,1.22564590575571,0.7));
#12293=CARTESIAN_POINT('Ctrl Pts',(2.78743249310418,1.23527907171202,0.7));
#12294=CARTESIAN_POINT('Ctrl Pts',(2.76507271635938,1.24261561512899,0.698430289974852));
#12295=CARTESIAN_POINT('Ctrl Pts',(2.73219941643314,1.24807722603274,0.696876198609429));
#12296=CARTESIAN_POINT('Ctrl Pts',(2.72335305886828,1.24906618730719,0.696525251810408));
#12297=CARTESIAN_POINT('Ctrl Pts',(2.71018695034311,1.24982905432238,0.696188910804419));
#12298=CARTESIAN_POINT('Ctrl Pts',(2.70590779780308,1.24996687586326,0.696107915309552));
#12299=CARTESIAN_POINT('Ctrl Pts',(2.69921702211412,1.25001037316246,0.696030339680738));
#12300=CARTESIAN_POINT('Ctrl Pts',(2.69680890442544,1.24999123464332,0.696012302673685));
#12301=CARTESIAN_POINT('Ctrl Pts',(2.69234597975348,1.24989125947742,0.695997601992606));
#12302=CARTESIAN_POINT('Ctrl Pts',(2.69029169500035,1.24981988388707,0.69599819279703));
#12303=CARTESIAN_POINT('Ctrl Pts',(2.6857660481318,1.24960673159635,0.696015705561832));
#12304=CARTESIAN_POINT('Ctrl Pts',(2.68329599580702,1.24945360531346,0.696035938105249));
#12305=CARTESIAN_POINT('Ctrl Pts',(2.67625328071593,1.24891193026541,0.696123377063474));
#12306=CARTESIAN_POINT('Ctrl Pts',(2.67169109188753,1.24843439216159,0.696216059649547));
#12307=CARTESIAN_POINT('Ctrl Pts',(2.64765560351845,1.24524789167778,0.696873729305584));
#12308=CARTESIAN_POINT('Ctrl Pts',(2.62857598726268,1.24037162800668,0.698048768812303));
#12309=CARTESIAN_POINT('Ctrl Pts',(2.59902076831046,1.22902239593109,0.699541037747764));
#12310=CARTESIAN_POINT('Ctrl Pts',(2.58799157881597,1.22383445108162,0.7));
#12311=CARTESIAN_POINT('Ctrl Pts',(2.57739843082979,1.21787348447436,0.7));
#12312=CARTESIAN_POINT('Origin',(2.7,1.,0.7));
#12313=CARTESIAN_POINT('Origin',(2.7,-1.,0.7));
#12314=CARTESIAN_POINT('',(2.57739843082979,-1.21787348447436,0.7));
#12315=CARTESIAN_POINT('',(2.80762864495888,-1.22564590575571,0.7));
#12316=CARTESIAN_POINT('Ctrl Pts',(2.57739843082979,-1.21787348447436,0.7));
#12317=CARTESIAN_POINT('Ctrl Pts',(2.59689796709118,-1.22884624579732,0.7));
#12318=CARTESIAN_POINT('Ctrl Pts',(2.61871070177046,-1.23767364961455,0.698430520021629));
#12319=CARTESIAN_POINT('Ctrl Pts',(2.6511387549791,-1.24533993869645,0.696876447160353));
#12320=CARTESIAN_POINT('Ctrl Pts',(2.65989793055836,-1.24692336726652,0.696525471319567));
#12321=CARTESIAN_POINT('Ctrl Pts',(2.67298219502323,-1.24857266139659,0.696189053183015));
#12322=CARTESIAN_POINT('Ctrl Pts',(2.67724223626036,-1.24899884484677,0.696108027479433));
#12323=CARTESIAN_POINT('Ctrl Pts',(2.68391475503581,-1.24949361628703,0.696030400846995));
#12324=CARTESIAN_POINT('Ctrl Pts',(2.68631866330158,-1.24963697932539,0.69601234479389));
#12325=CARTESIAN_POINT('Ctrl Pts',(2.69077815115796,-1.24983831390468,0.695997608323079));
#12326=CARTESIAN_POINT('Ctrl Pts',(2.69283257145917,-1.24990568929416,0.695998182544699));
#12327=CARTESIAN_POINT('Ctrl Pts',(2.69736230434386,-1.24999833696454,0.696015659042177));
#12328=CARTESIAN_POINT('Ctrl Pts',(2.69983707579759,-1.25001219669429,0.696035872086962));
#12329=CARTESIAN_POINT('Ctrl Pts',(2.70690037992806,-1.24994687665095,0.696123257636812));
#12330=CARTESIAN_POINT('Ctrl Pts',(2.71148446565418,-1.24977820005943,0.696215908504701));
#12331=CARTESIAN_POINT('Ctrl Pts',(2.73568105999059,-1.24822038288304,0.696873447340259));
#12332=CARTESIAN_POINT('Ctrl Pts',(2.75504695022812,-1.24464213141243,0.698048515307351));
#12333=CARTESIAN_POINT('Ctrl Pts',(2.78530198112344,-1.2353118289445,0.699540950501024));
#12334=CARTESIAN_POINT('Ctrl Pts',(2.79665680001786,-1.23087925931356,0.7));
#12335=CARTESIAN_POINT('Ctrl Pts',(2.80762864495888,-1.22564590575571,0.7));
#12336=CARTESIAN_POINT('Origin',(2.7,-1.,0.7));
#12337=CARTESIAN_POINT('Origin',(8.1,1.,0.7));
#12338=CARTESIAN_POINT('',(8.26514540988519,1.18768855477586,0.7));
#12339=CARTESIAN_POINT('',(7.94916965249954,1.19937453719419,0.7));
#12340=CARTESIAN_POINT('Ctrl Pts',(8.26514540988519,1.18768855477586,0.7));
#12341=CARTESIAN_POINT('Ctrl Pts',(8.24402114884725,1.20627559516199,0.7));
#12342=CARTESIAN_POINT('Ctrl Pts',(8.21930102059268,1.22168408824046,0.695284768760077));
#12343=CARTESIAN_POINT('Ctrl Pts',(8.17833936508797,1.23784683595578,0.688517484674842));
#12344=CARTESIAN_POINT('Ctrl Pts',(8.16442627443898,1.24199461640617,0.686388979601913));
#12345=CARTESIAN_POINT('Ctrl Pts',(8.14282164862934,1.24641910835203,0.684139556285851));
#12346=CARTESIAN_POINT('Ctrl Pts',(8.13541969045672,1.24759243465272,0.683546718614312));
#12347=CARTESIAN_POINT('Ctrl Pts',(8.12445132655127,1.24882623938238,0.682995554842566));
#12348=CARTESIAN_POINT('Ctrl Pts',(8.12094947916695,1.24914555886372,0.68286756899844));
#12349=CARTESIAN_POINT('Ctrl Pts',(8.11555178799172,1.24952297970176,0.682747494033431));
#12350=CARTESIAN_POINT('Ctrl Pts',(8.11366421100955,1.24963346420394,0.682719937279798));
#12351=CARTESIAN_POINT('Ctrl Pts',(8.11020620287515,1.24979651712922,0.682696124556263));
#12352=CARTESIAN_POINT('Ctrl Pts',(8.10863696767328,1.24985569708818,0.682695355189016));
#12353=CARTESIAN_POINT('Ctrl Pts',(8.10522484403353,1.249952190393,0.682715496638402));
#12354=CARTESIAN_POINT('Ctrl Pts',(8.10338263267786,1.24998390529834,0.682740187713169));
#12355=CARTESIAN_POINT('Ctrl Pts',(8.09833277498968,1.25001501472208,0.682845394223802));
#12356=CARTESIAN_POINT('Ctrl Pts',(8.09512844909059,1.24997307323179,0.682953673497893));
#12357=CARTESIAN_POINT('Ctrl Pts',(8.07918314804204,1.24945780552822,0.683691186949858));
#12358=CARTESIAN_POINT('Ctrl Pts',(8.06659630270856,1.24808001426183,0.684918585227095));
#12359=CARTESIAN_POINT('Ctrl Pts',(8.02558960427868,1.24043495378573,0.69021260546313));
#12360=CARTESIAN_POINT('Ctrl Pts',(7.9986188553413,1.2302509517108,0.695754623970086));
#12361=CARTESIAN_POINT('Ctrl Pts',(7.96559475436581,1.21103543221342,0.69939729083119));
#12362=CARTESIAN_POINT('Ctrl Pts',(7.95720051358587,1.20545002552208,0.7));
#12363=CARTESIAN_POINT('Ctrl Pts',(7.94916965151797,1.19937453693185,0.7));
#12364=CARTESIAN_POINT('Origin',(8.1,1.,0.7));
#12365=CARTESIAN_POINT('Ctrl Pts',(1.1,1.14549341399196,0.7));
#12366=CARTESIAN_POINT('Ctrl Pts',(1.89984199608574,1.1957170361627,0.7));
#12367=CARTESIAN_POINT('Ctrl Pts',(2.70080437300401,1.2273695200909,0.7));
#12368=CARTESIAN_POINT('Ctrl Pts',(3.50204003610941,1.24374118183538,0.7));
#12369=CARTESIAN_POINT('Ctrl Pts',(1.09819048660397,1.17431102498992,0.7));
#12370=CARTESIAN_POINT('Ctrl Pts',(1.89847848223077,1.22458382597074,0.70000077422621));
#12371=CARTESIAN_POINT('Ctrl Pts',(2.69984520196781,1.25626413437997,0.699999727319846));
#12372=CARTESIAN_POINT('Ctrl Pts',(3.50144932661635,1.27265074030048,0.700000000000001));
#12373=CARTESIAN_POINT('Ctrl Pts',(1.09505363188407,1.22426736091617,0.676703190608825));
#12374=CARTESIAN_POINT('Ctrl Pts',(1.89610976425884,1.27462253270773,0.67666760713801));
#12375=CARTESIAN_POINT('Ctrl Pts',(2.69818680938115,1.3063522351595,0.67664530655333));
#12376=CARTESIAN_POINT('Ctrl Pts',(3.50042536655637,1.322763754511,0.676632802377821));
#12377=CARTESIAN_POINT('Ctrl Pts',(1.09381704710221,1.24396073223232,0.627109609335854));
#12378=CARTESIAN_POINT('Ctrl Pts',(1.89518106151152,1.29430885982199,0.62701751976321));
#12379=CARTESIAN_POINT('Ctrl Pts',(2.69753328610131,1.32603127467068,0.626959208652505));
#12380=CARTESIAN_POINT('Ctrl Pts',(3.50002334924346,1.34243864233338,0.626926882269943));
#12381=CARTESIAN_POINT('Ctrl Pts',(1.09374258853658,1.24514653057163,0.605486452199395));
#12382=CARTESIAN_POINT('Ctrl Pts',(1.89512529323683,1.29547288309274,0.605377720397184));
#12383=CARTESIAN_POINT('Ctrl Pts',(2.69749615303001,1.32718177535833,0.605308474776761));
#12384=CARTESIAN_POINT('Ctrl Pts',(3.5,1.34358136363184,0.605270327458635));
#12385=CARTESIAN_POINT('',(1.1,1.14549341399195,0.7));
#12386=CARTESIAN_POINT('Ctrl Pts',(1.1,1.14549341399196,0.7));
#12387=CARTESIAN_POINT('Ctrl Pts',(1.59210562457523,1.17639367564078,0.7));
#12388=CARTESIAN_POINT('Ctrl Pts',(2.08463535466703,1.20026407570248,0.7));
#12389=CARTESIAN_POINT('Ctrl Pts',(2.57739190516306,1.2178709162388,0.7));
#12390=CARTESIAN_POINT('',(1.1,1.24553911298206,0.605485603995113));
#12391=CARTESIAN_POINT('Ctrl Pts',(1.1,1.14549341399196,0.7));
#12392=CARTESIAN_POINT('Ctrl Pts',(1.1,1.15341616150799,0.7));
#12393=CARTESIAN_POINT('Ctrl Pts',(1.1000012416168,1.16127613060545,0.699006361583129));
#12394=CARTESIAN_POINT('Ctrl Pts',(1.10000231308998,1.16893252943985,0.697119293189023));
#12395=CARTESIAN_POINT('Ctrl Pts',(1.10000291357081,1.17322337016277,0.696061732044743));
#12396=CARTESIAN_POINT('Ctrl Pts',(1.10000345673767,1.17745032641463,0.694722535963768));
#12397=CARTESIAN_POINT('Ctrl Pts',(1.10000379529503,1.18158693416151,0.693112479763539));
#12398=CARTESIAN_POINT('Ctrl Pts',(1.1000044034764,1.18901789868739,0.690220189452084));
#12399=CARTESIAN_POINT('Ctrl Pts',(1.1000042334852,1.19607766167095,0.686488065947256));
#12400=CARTESIAN_POINT('Ctrl Pts',(1.10000339376692,1.2026196529327,0.681996646156542));
#12401=CARTESIAN_POINT('Ctrl Pts',(1.10000293249552,1.20621327895058,0.67952943359521));
#12402=CARTESIAN_POINT('Ctrl Pts',(1.10000228571683,1.20965039763183,0.676832226278619));
#12403=CARTESIAN_POINT('Ctrl Pts',(1.10000171524363,1.21290279159005,0.673912896410569));
#12404=CARTESIAN_POINT('Ctrl Pts',(1.10000115816795,1.2160788033717,0.671062126739188));
#12405=CARTESIAN_POINT('Ctrl Pts',(1.10000066850715,1.2190594221245,0.668016750164662));
#12406=CARTESIAN_POINT('Ctrl Pts',(1.10000067525152,1.22182202639256,0.664788091882127));
#12407=CARTESIAN_POINT('Ctrl Pts',(1.10000068775799,1.22694487635592,0.658801012170571));
#12408=CARTESIAN_POINT('Ctrl Pts',(1.10000222199399,1.23132099043293,0.652185071179834));
#12409=CARTESIAN_POINT('Ctrl Pts',(1.10000276904041,1.23488987417606,0.64510534613808));
#12410=CARTESIAN_POINT('Ctrl Pts',(1.10000282439334,1.23525099193115,0.644388983656765));
#12411=CARTESIAN_POINT('Ctrl Pts',(1.10000287212626,1.23560380546488,0.64366785367332));
#12412=CARTESIAN_POINT('Ctrl Pts',(1.10000291138002,1.23594822450451,0.642942116631622));
#12413=CARTESIAN_POINT('Ctrl Pts',(1.10000329911404,1.23935026814133,0.635773555081239));
#12414=CARTESIAN_POINT('Ctrl Pts',(1.10000258010782,1.24189771450306,0.628240464257889));
#12415=CARTESIAN_POINT('Ctrl Pts',(1.10000149084855,1.24353681278199,0.620511076118615));
#12416=CARTESIAN_POINT('Ctrl Pts',(1.10000079446814,1.24458471384188,0.615569557890241));
#12417=CARTESIAN_POINT('Ctrl Pts',(1.10000000111128,1.24526049271905,0.610547146027233));
#12418=CARTESIAN_POINT('Ctrl Pts',(1.09999999916631,1.24553911263843,0.605485603997432));
#12419=CARTESIAN_POINT('',(3.5,1.34358136363184,0.605270327458635));
#12420=CARTESIAN_POINT('Ctrl Pts',(3.5,1.34358136363184,0.605270327458635));
#12421=CARTESIAN_POINT('Ctrl Pts',(2.6995848679345,1.32722445934619,0.605308375488923));
#12422=CARTESIAN_POINT('Ctrl Pts',(1.89930203168261,1.29563783986497,0.605377360150118));
#12423=CARTESIAN_POINT('Ctrl Pts',(1.09999999916631,1.24553911263843,0.605485603997431));
#12424=CARTESIAN_POINT('',(3.5,1.24369946473792,0.7));
#12425=CARTESIAN_POINT('Ctrl Pts',(3.5,1.34358136363184,0.605270327458635));
#12426=CARTESIAN_POINT('Ctrl Pts',(3.5,1.34316359984937,0.613184373088104));
#12427=CARTESIAN_POINT('Ctrl Pts',(3.50000057901142,1.34177887744868,0.621008021569537));
#12428=CARTESIAN_POINT('Ctrl Pts',(3.50000082863025,1.33951086762262,0.628580534231506));
#12429=CARTESIAN_POINT('Ctrl Pts',(3.50000096811,1.33824356956914,0.632811834486987));
#12430=CARTESIAN_POINT('Ctrl Pts',(3.50000102536574,1.33669948631919,0.636964759527324));
#12431=CARTESIAN_POINT('Ctrl Pts',(3.50000098105742,1.334886463945,0.641009258704104));
#12432=CARTESIAN_POINT('Ctrl Pts',(3.50000090179773,1.3316432906201,0.648244145614236));
#12433=CARTESIAN_POINT('Ctrl Pts',(3.50000044940971,1.3275777080273,0.655054131048541));
#12434=CARTESIAN_POINT('Ctrl Pts',(3.50000027423476,1.32275302640998,0.661275670751788));
#12435=CARTESIAN_POINT('Ctrl Pts',(3.50000024156065,1.32185311357394,0.66243612938574));
#12436=CARTESIAN_POINT('Ctrl Pts',(3.50000022115524,1.32092666334894,0.663576045687695));
#12437=CARTESIAN_POINT('Ctrl Pts',(3.50000022069074,1.31997391848392,0.664694242102532));
#12438=CARTESIAN_POINT('Ctrl Pts',(3.50000021976176,1.31806844339147,0.666930617752677));
#12439=CARTESIAN_POINT('Ctrl Pts',(3.50000029790302,1.31605782519,0.669080165434128));
#12440=CARTESIAN_POINT('Ctrl Pts',(3.50000040488465,1.31394946763378,0.671139079687271));
#12441=CARTESIAN_POINT('Ctrl Pts',(3.50000069329649,1.3082655455861,0.6766897075128));
#12442=CARTESIAN_POINT('Ctrl Pts',(3.5000011432336,1.30193818666762,0.681521899278667));
#12443=CARTESIAN_POINT('Ctrl Pts',(3.50000129797765,1.29513115062548,0.68558123547136));
#12444=CARTESIAN_POINT('Ctrl Pts',(3.50000139624096,1.2908086457691,0.688158936000333));
#12445=CARTESIAN_POINT('Ctrl Pts',(3.50000139493488,1.28629176508013,0.690424313967808));
#12446=CARTESIAN_POINT('Ctrl Pts',(3.50000129141552,1.28161680488022,0.692354162840695));
#12447=CARTESIAN_POINT('Ctrl Pts',(3.50000112941005,1.27430059661786,0.695374333209024));
#12448=CARTESIAN_POINT('Ctrl Pts',(3.5000007162179,1.26668229982361,0.697540280949125));
#12449=CARTESIAN_POINT('Ctrl Pts',(3.50000038344698,1.25890895215876,0.698782355543395));
#12450=CARTESIAN_POINT('Ctrl Pts',(3.50000016866387,1.25389173534334,0.699584038140014));
#12451=CARTESIAN_POINT('Ctrl Pts',(3.4999999993056,1.24880933504677,0.69999999987784));
#12452=CARTESIAN_POINT('Ctrl Pts',(3.49999999991873,1.24369946470729,0.7));
#12453=CARTESIAN_POINT('Ctrl Pts',(2.80762377174497,1.22564400643366,0.7));
#12454=CARTESIAN_POINT('Ctrl Pts',(3.03837960601223,1.23298334400942,0.7));
#12455=CARTESIAN_POINT('Ctrl Pts',(3.26917843294065,1.23897560812206,0.7));
#12456=CARTESIAN_POINT('Ctrl Pts',(3.49999999991873,1.24369946470729,0.7));
#12457=CARTESIAN_POINT('Ctrl Pts',(7.29709043526678,1.22049830417059,0.7));
#12458=CARTESIAN_POINT('Ctrl Pts',(8.19846709497879,1.19422430779862,0.7));
#12459=CARTESIAN_POINT('Ctrl Pts',(9.09944331332256,1.15544418981837,0.7));
#12460=CARTESIAN_POINT('Ctrl Pts',(10.,1.10900986674273,0.7));
#12461=CARTESIAN_POINT('Ctrl Pts',(7.29793284700474,1.24939875264889,0.7));
#12462=CARTESIAN_POINT('Ctrl Pts',(8.19957769811722,1.22310890030201,0.699999704549177));
#12463=CARTESIAN_POINT('Ctrl Pts',(9.10076698492607,1.18430758604571,0.700000491839571));
#12464=CARTESIAN_POINT('Ctrl Pts',(10.0014871213396,1.13785139984992,0.7));
#12465=CARTESIAN_POINT('Ctrl Pts',(7.29939288958794,1.29948813715084,0.676630595533454));
#12466=CARTESIAN_POINT('Ctrl Pts',(8.20149954052228,1.27317186922949,0.676644146017132));
#12467=CARTESIAN_POINT('Ctrl Pts',(9.10306300621911,1.23433322993607,0.676664155483857));
#12468=CARTESIAN_POINT('Ctrl Pts',(10.0040646682326,1.18784086746588,0.676686753673613));
#12469=CARTESIAN_POINT('Ctrl Pts',(7.29996660609513,1.31917051289423,0.626939603849942));
#12470=CARTESIAN_POINT('Ctrl Pts',(8.20225661204673,1.29285896783792,0.626974637782525));
#12471=CARTESIAN_POINT('Ctrl Pts',(9.10396596140606,1.25402923300358,0.627026849623412));
#12472=CARTESIAN_POINT('Ctrl Pts',(10.0050807923581,1.20754778500352,0.627085325222079));
#12473=CARTESIAN_POINT('Ctrl Pts',(7.29999999953093,1.32031613471704,0.605285370449856));
#12474=CARTESIAN_POINT('Ctrl Pts',(8.20230020786565,1.29401302889245,0.605326714446839));
#12475=CARTESIAN_POINT('Ctrl Pts',(9.10401978846669,1.25519559703033,0.605388684776982));
#12476=CARTESIAN_POINT('Ctrl Pts',(10.0051416645797,1.20872835322339,0.605457722909465));
#12477=CARTESIAN_POINT('',(7.29999999989017,1.22041345054104,0.7));
#12478=CARTESIAN_POINT('Ctrl Pts',(7.29999999978094,1.22041345055303,0.7));
#12479=CARTESIAN_POINT('Ctrl Pts',(7.51641201913776,1.21409884615949,0.7));
#12480=CARTESIAN_POINT('Ctrl Pts',(7.73280095443524,1.20706364503479,0.7));
#12481=CARTESIAN_POINT('Ctrl Pts',(7.94916654146952,1.19937499621344,0.7));
#12482=CARTESIAN_POINT('',(7.29999999953133,1.3203161347307,0.605285370449834));
#12483=CARTESIAN_POINT('Ctrl Pts',(7.29999999989087,1.22041345054982,0.7));
#12484=CARTESIAN_POINT('Ctrl Pts',(7.30000000079355,1.22832360919786,0.699999999740221));
#12485=CARTESIAN_POINT('Ctrl Pts',(7.29999941101664,1.23617007614594,0.699006006469939));
#12486=CARTESIAN_POINT('Ctrl Pts',(7.29999889581476,1.24381267896118,0.697118889344366));
#12487=CARTESIAN_POINT('Ctrl Pts',(7.29999860583198,1.24811433880851,0.696056720321257));
#12488=CARTESIAN_POINT('Ctrl Pts',(7.29999834128398,1.25235147078274,0.694710570513598));
#12489=CARTESIAN_POINT('Ctrl Pts',(7.29999817264931,1.25649739217805,0.693091458416622));
#12490=CARTESIAN_POINT('Ctrl Pts',(7.29999787070862,1.26392067210813,0.690192435210923));
#12491=CARTESIAN_POINT('Ctrl Pts',(7.29999793286912,1.27097116792553,0.686452948287278));
#12492=CARTESIAN_POINT('Ctrl Pts',(7.2999983123982,1.27750284616821,0.681954753865011));
#12493=CARTESIAN_POINT('Ctrl Pts',(7.2999985213788,1.28109939299731,0.679477906983553));
#12494=CARTESIAN_POINT('Ctrl Pts',(7.29999881895966,1.28453837241868,0.676770138671336));
#12495=CARTESIAN_POINT('Ctrl Pts',(7.29999908362886,1.28779148632494,0.673839551409954));
#12496=CARTESIAN_POINT('Ctrl Pts',(7.29999934163235,1.29096267037196,0.670982771155867));
#12497=CARTESIAN_POINT('Ctrl Pts',(7.29999957112158,1.2939379836903,0.667931525418885));
#12498=CARTESIAN_POINT('Ctrl Pts',(7.29999957127586,1.29669488996436,0.664697318929259));
#12499=CARTESIAN_POINT('Ctrl Pts',(7.29999957156178,1.30180432468448,0.658703293276094));
#12500=CARTESIAN_POINT('Ctrl Pts',(7.29999886995656,1.30616650855536,0.652082235935803));
#12501=CARTESIAN_POINT('Ctrl Pts',(7.29999863193158,1.30972187224872,0.644999691185358));
#12502=CARTESIAN_POINT('Ctrl Pts',(7.29999860759325,1.31008541227461,0.644275492840527));
#12503=CARTESIAN_POINT('Ctrl Pts',(7.29999858692673,1.31044047656777,0.643546449710686));
#12504=CARTESIAN_POINT('Ctrl Pts',(7.29999857034625,1.31078697300061,0.642812727646596));
#12505=CARTESIAN_POINT('Ctrl Pts',(7.29999840819729,1.31417553742296,0.635637287305567));
#12506=CARTESIAN_POINT('Ctrl Pts',(7.29999876577208,1.31670951795567,0.628098908385918));
#12507=CARTESIAN_POINT('Ctrl Pts',(7.29999928780719,1.3183355664444,0.620365998324013));
#12508=CARTESIAN_POINT('Ctrl Pts',(7.29999962266353,1.3193785856694,0.615405768714856));
#12509=CARTESIAN_POINT('Ctrl Pts',(7.3,1.32004717656055,0.610364828659741));
#12510=CARTESIAN_POINT('Ctrl Pts',(7.3,1.32031613470337,0.605285370449877));
#12511=CARTESIAN_POINT('',(10.,1.20899340483173,0.605457329065657));
#12512=CARTESIAN_POINT('Ctrl Pts',(9.99999999968202,1.20899340489109,0.605457329065633));
#12513=CARTESIAN_POINT('Ctrl Pts',(9.10058974048747,1.25534320916473,0.605388449123016));
#12514=CARTESIAN_POINT('Ctrl Pts',(8.20058408060299,1.29406305600824,0.605326635812744));
#12515=CARTESIAN_POINT('Ctrl Pts',(7.29999999953093,1.32031613471704,0.605285370449856));
#12516=CARTESIAN_POINT('',(9.99999999523418,1.1090098672342,0.7));
#12517=CARTESIAN_POINT('Ctrl Pts',(9.99999999968202,1.20899340489109,0.605457329065633));
#12518=CARTESIAN_POINT('Ctrl Pts',(9.99999999887489,1.20856043137698,0.613368813757176));
#12519=CARTESIAN_POINT('Ctrl Pts',(9.99999852309337,1.20715974444566,0.621187403383205));
#12520=CARTESIAN_POINT('Ctrl Pts',(9.99999786661901,1.20487567413208,0.628752957409046));
#12521=CARTESIAN_POINT('Ctrl Pts',(9.9999975031266,1.20361097553651,0.63294203403));
#12522=CARTESIAN_POINT('Ctrl Pts',(9.99999733971606,1.20207445367248,0.63705356322819));
#12523=CARTESIAN_POINT('Ctrl Pts',(9.99999742766416,1.20027388348257,0.64105842070465));
#12524=CARTESIAN_POINT('Ctrl Pts',(9.9999975865154,1.19702170610966,0.6482919664668));
#12525=CARTESIAN_POINT('Ctrl Pts',(9.99999868569093,1.19294650045069,0.655099368158521));
#12526=CARTESIAN_POINT('Ctrl Pts',(9.9999991134218,1.18811276085989,0.661317774786376));
#12527=CARTESIAN_POINT('Ctrl Pts',(9.99999919410111,1.18720101282252,0.662490701033652));
#12528=CARTESIAN_POINT('Ctrl Pts',(9.99999924414009,1.18626214680169,0.663642601192937));
#12529=CARTESIAN_POINT('Ctrl Pts',(9.99999924372355,1.18529642131707,0.664772262763739));
#12530=CARTESIAN_POINT('Ctrl Pts',(9.99999924291654,1.18342543943696,0.666960851926287));
#12531=CARTESIAN_POINT('Ctrl Pts',(9.99999905429896,1.18145367213587,0.669066014649603));
#12532=CARTESIAN_POINT('Ctrl Pts',(9.99999879621773,1.17938809187152,0.671084194359814));
#12533=CARTESIAN_POINT('Ctrl Pts',(9.99999808597787,1.17370361260899,0.676638227242868));
#12534=CARTESIAN_POINT('Ctrl Pts',(9.9999969699445,1.16737553754052,0.681473799108647));
#12535=CARTESIAN_POINT('Ctrl Pts',(9.99999660204079,1.16056788011185,0.685537070165577));
#12536=CARTESIAN_POINT('Ctrl Pts',(9.99999636768906,1.15623145667386,0.688125341392612));
#12537=CARTESIAN_POINT('Ctrl Pts',(9.99999638726733,1.15169947441128,0.690399565850749));
#12538=CARTESIAN_POINT('Ctrl Pts',(9.99999666360534,1.14700857532255,0.692336497939236));
#12539=CARTESIAN_POINT('Ctrl Pts',(9.99999709503399,1.13968497812548,0.695360504669253));
#12540=CARTESIAN_POINT('Ctrl Pts',(9.99999815490668,1.13205884654683,0.697530003145419));
#12541=CARTESIAN_POINT('Ctrl Pts',(9.99999900983214,1.12427739544825,0.698775573347137));
#12542=CARTESIAN_POINT('Ctrl Pts',(9.99999956314479,1.11924119569193,0.699581713521624));
#12543=CARTESIAN_POINT('Ctrl Pts',(10.,1.11413933950174,0.7));
#12544=CARTESIAN_POINT('Ctrl Pts',(10.,1.10900986674273,0.7));
#12545=CARTESIAN_POINT('Ctrl Pts',(8.26514054272776,1.18768929227839,0.7));
#12546=CARTESIAN_POINT('Ctrl Pts',(8.84359655063997,1.16547286645366,0.7));
#12547=CARTESIAN_POINT('Ctrl Pts',(9.42188471826001,1.13881853081542,0.7));
#12548=CARTESIAN_POINT('Ctrl Pts',(9.99999999522154,1.10900986698912,0.7));
#12549=CARTESIAN_POINT('Origin',(5.4,-8.11656130105013E-18,0.7));
#12550=CARTESIAN_POINT('',(7.3,-1.22041345053557,0.7));
#12551=CARTESIAN_POINT('Ctrl Pts',(7.94916654049851,-1.19937499624794,0.7));
#12552=CARTESIAN_POINT('Ctrl Pts',(7.73280095382446,-1.20706364505454,0.7));
#12553=CARTESIAN_POINT('Ctrl Pts',(7.51641201888728,-1.21409884616656,0.7));
#12554=CARTESIAN_POINT('Ctrl Pts',(7.29999999989085,-1.22041345054982,0.7));
#12555=CARTESIAN_POINT('',(7.3,-0.712777777777778,0.7));
#12556=CARTESIAN_POINT('',(10.,-1.10900986674244,0.7));
#12557=CARTESIAN_POINT('',(10.,0.653773457742722,0.7));
#12558=CARTESIAN_POINT('Ctrl Pts',(10.,-1.10900986674273,0.7));
#12559=CARTESIAN_POINT('Ctrl Pts',(9.42188472144661,-1.13881853066854,0.7));
#12560=CARTESIAN_POINT('Ctrl Pts',(8.84359655223373,-1.16547286639245,0.7));
#12561=CARTESIAN_POINT('Ctrl Pts',(8.26514054272776,-1.18768929227839,0.7));
#12562=CARTESIAN_POINT('',(7.95,-1.,0.7));
#12563=CARTESIAN_POINT('Origin',(8.1,-1.,0.7));
#12564=CARTESIAN_POINT('',(7.95,1.,0.7));
#12565=CARTESIAN_POINT('Origin',(8.1,1.,0.7));
#12566=CARTESIAN_POINT('',(8.4,-4.89858719658942E-17,0.7));
#12567=CARTESIAN_POINT('Origin',(8.8,0.,0.7));
#12568=CARTESIAN_POINT('Origin',(8.1,-1.,0.8));
#12569=CARTESIAN_POINT('',(7.95,-1.,0.9));
#12570=CARTESIAN_POINT('Origin',(8.1,-1.,0.9));
#12571=CARTESIAN_POINT('',(7.95,-1.,0.8));
#12572=CARTESIAN_POINT('Origin',(2.7,-1.,0.8));
#12573=CARTESIAN_POINT('',(2.55,-1.,0.9));
#12574=CARTESIAN_POINT('Origin',(2.7,-1.,0.9));
#12575=CARTESIAN_POINT('',(2.55,-1.,0.7));
#12576=CARTESIAN_POINT('',(2.55,-1.,0.8));
#12577=CARTESIAN_POINT('Origin',(2.7,-1.,0.7));
#12578=CARTESIAN_POINT('Origin',(2.7,1.,0.8));
#12579=CARTESIAN_POINT('',(2.55,1.,0.9));
#12580=CARTESIAN_POINT('Origin',(2.7,1.,0.9));
#12581=CARTESIAN_POINT('',(2.55,1.,0.7));
#12582=CARTESIAN_POINT('',(2.55,1.,0.8));
#12583=CARTESIAN_POINT('Origin',(2.7,1.,0.7));
#12584=CARTESIAN_POINT('Origin',(8.1,1.,0.8));
#12585=CARTESIAN_POINT('',(7.95,1.,0.9));
#12586=CARTESIAN_POINT('Origin',(8.1,1.,0.9));
#12587=CARTESIAN_POINT('',(7.95,1.,0.8));
#12588=CARTESIAN_POINT('Origin',(2.,0.,0.75));
#12589=CARTESIAN_POINT('',(1.7,3.67394039744206E-17,0.9));
#12590=CARTESIAN_POINT('Origin',(2.,0.,0.9));
#12591=CARTESIAN_POINT('',(1.7,3.67394039744206E-17,0.6));
#12592=CARTESIAN_POINT('',(1.7,3.67394039744206E-17,0.75));
#12593=CARTESIAN_POINT('Origin',(2.,0.,0.6));
#12594=CARTESIAN_POINT('Origin',(2.,0.,0.6));
#12595=CARTESIAN_POINT('',(1.83,-2.0818995585505E-17,0.6));
#12596=CARTESIAN_POINT('Origin',(2.,0.,0.6));
#12597=CARTESIAN_POINT('Origin',(8.8,0.,0.75));
#12598=CARTESIAN_POINT('',(8.5,3.67394039744206E-17,0.9));
#12599=CARTESIAN_POINT('Origin',(8.8,0.,0.9));
#12600=CARTESIAN_POINT('',(8.5,3.67394039744206E-17,0.6));
#12601=CARTESIAN_POINT('',(8.5,3.67394039744206E-17,0.75));
#12602=CARTESIAN_POINT('Origin',(8.8,0.,0.6));
#12603=CARTESIAN_POINT('Origin',(8.8,0.,0.6));
#12604=CARTESIAN_POINT('',(8.63,-2.0818995585505E-17,0.6));
#12605=CARTESIAN_POINT('Origin',(8.8,0.,0.6));
#12606=CARTESIAN_POINT('Origin',(2.,0.,0.45));
#12607=CARTESIAN_POINT('',(1.83,-2.0818995585505E-17,0.32));
#12608=CARTESIAN_POINT('',(1.83,2.0818995585505E-17,0.45));
#12609=CARTESIAN_POINT('Origin',(2.,0.,0.32));
#12610=CARTESIAN_POINT('Origin',(8.8,0.,0.45));
#12611=CARTESIAN_POINT('',(8.63,-2.0818995585505E-17,0.32));
#12612=CARTESIAN_POINT('',(8.63,2.0818995585505E-17,0.45));
#12613=CARTESIAN_POINT('Origin',(8.8,0.,0.32));
#12614=CARTESIAN_POINT('Origin',(10.,-0.62,0.32));
#12615=CARTESIAN_POINT('',(0.200274469199584,-0.62,0.));
#12616=CARTESIAN_POINT('',(0.217044958570157,-0.62,0.32));
#12617=CARTESIAN_POINT('',(0.221783445591644,-0.62,0.410415718550007));
#12618=CARTESIAN_POINT('',(0.,-0.62,0.));
#12619=CARTESIAN_POINT('',(7.7,-0.62,0.));
#12620=CARTESIAN_POINT('',(0.0167704893705732,-0.62,0.32));
#12621=CARTESIAN_POINT('',(0.0220575386407278,-0.62,0.420882909798596));
#12622=CARTESIAN_POINT('',(-0.1,-0.62,0.32));
#12623=CARTESIAN_POINT('Origin',(10.,-0.62,0.32));
#12624=CARTESIAN_POINT('',(0.9,-0.62,0.32));
#12625=CARTESIAN_POINT('',(0.9,-0.62,0.));
#12626=CARTESIAN_POINT('',(0.9,-0.62,0.16));
#12627=CARTESIAN_POINT('',(1.1,-0.62,0.32));
#12628=CARTESIAN_POINT('',(-0.1,-0.62,0.32));
#12629=CARTESIAN_POINT('',(1.1,-0.62,0.));
#12630=CARTESIAN_POINT('',(1.1,-0.62,0.16));
#12631=CARTESIAN_POINT('',(7.7,-0.62,0.));
#12632=CARTESIAN_POINT('Origin',(10.,-0.62,0.32));
#12633=CARTESIAN_POINT('',(3.5,-0.62,0.32));
#12634=CARTESIAN_POINT('',(3.5,-0.62,0.));
#12635=CARTESIAN_POINT('',(3.5,-0.62,0.16));
#12636=CARTESIAN_POINT('',(3.7,-0.62,0.32));
#12637=CARTESIAN_POINT('',(-0.1,-0.62,0.32));
#12638=CARTESIAN_POINT('',(3.7,-0.62,0.));
#12639=CARTESIAN_POINT('',(3.7,-0.62,0.16));
#12640=CARTESIAN_POINT('',(7.7,-0.62,0.));
#12641=CARTESIAN_POINT('Origin',(10.,-0.62,0.32));
#12642=CARTESIAN_POINT('',(7.1,-0.62,0.32));
#12643=CARTESIAN_POINT('',(7.1,-0.62,0.));
#12644=CARTESIAN_POINT('',(7.1,-0.62,0.16));
#12645=CARTESIAN_POINT('',(7.3,-0.62,0.32));
#12646=CARTESIAN_POINT('',(-0.1,-0.62,0.32));
#12647=CARTESIAN_POINT('',(7.3,-0.62,0.));
#12648=CARTESIAN_POINT('',(7.3,-0.62,0.16));
#12649=CARTESIAN_POINT('',(7.7,-0.62,0.));
#12650=CARTESIAN_POINT('Origin',(-0.0999999999999996,0.62,0.32));
#12651=CARTESIAN_POINT('',(0.217044958570158,0.62,0.32));
#12652=CARTESIAN_POINT('',(0.200274469199584,0.62,0.));
#12653=CARTESIAN_POINT('',(0.207951231396534,0.62,0.146481348799182));
#12654=CARTESIAN_POINT('',(0.0167704893705736,0.62,0.32));
#12655=CARTESIAN_POINT('',(10.,0.62,0.32));
#12656=CARTESIAN_POINT('',(0.,0.62,0.));
#12657=CARTESIAN_POINT('',(0.00822532444561912,0.62,0.156948540047771));
#12658=CARTESIAN_POINT('',(2.65,0.62,0.));
#12659=CARTESIAN_POINT('Origin',(-0.0999999999999996,0.62,0.32));
#12660=CARTESIAN_POINT('',(0.9,0.62,0.));
#12661=CARTESIAN_POINT('',(0.9,0.62,0.32));
#12662=CARTESIAN_POINT('',(0.9,0.62,0.16));
#12663=CARTESIAN_POINT('',(1.1,0.62,0.));
#12664=CARTESIAN_POINT('',(2.65,0.62,0.));
#12665=CARTESIAN_POINT('',(1.1,0.62,0.32));
#12666=CARTESIAN_POINT('',(1.1,0.62,0.16));
#12667=CARTESIAN_POINT('',(10.,0.62,0.32));
#12668=CARTESIAN_POINT('Origin',(-0.0999999999999996,0.62,0.32));
#12669=CARTESIAN_POINT('',(3.5,0.62,0.));
#12670=CARTESIAN_POINT('',(3.5,0.62,0.32));
#12671=CARTESIAN_POINT('',(3.5,0.62,0.16));
#12672=CARTESIAN_POINT('',(3.7,0.62,0.));
#12673=CARTESIAN_POINT('',(2.65,0.62,0.));
#12674=CARTESIAN_POINT('',(3.7,0.62,0.32));
#12675=CARTESIAN_POINT('',(3.7,0.62,0.16));
#12676=CARTESIAN_POINT('',(10.,0.62,0.32));
#12677=CARTESIAN_POINT('Origin',(4.95,0.,0.32));
#12678=CARTESIAN_POINT('',(1.6,-4.89858719658941E-17,0.32));
#12679=CARTESIAN_POINT('Origin',(2.,0.,0.32));
#12680=CARTESIAN_POINT('Origin',(4.95,0.,0.32));
#12681=CARTESIAN_POINT('',(8.4,-4.89858719658942E-17,0.32));
#12682=CARTESIAN_POINT('Origin',(8.8,0.,0.32));
#12683=CARTESIAN_POINT('Origin',(4.95,0.,0.32));
#12684=CARTESIAN_POINT('',(0.217044958570157,-0.7,0.32));
#12685=CARTESIAN_POINT('',(0.0167704893705731,-0.7,0.32));
#12686=CARTESIAN_POINT('Origin',(4.95,0.,0.32));
#12687=CARTESIAN_POINT('',(0.9,0.671641708581009,0.32));
#12688=CARTESIAN_POINT('',(1.1,-0.671641708581009,0.32));
#12689=CARTESIAN_POINT('Origin',(4.95,0.,0.32));
#12690=CARTESIAN_POINT('',(3.5,0.723888888888889,0.32));
#12691=CARTESIAN_POINT('',(3.7,-0.723888888888889,0.32));
#12692=CARTESIAN_POINT('Origin',(4.95,0.,0.32));
#12693=CARTESIAN_POINT('',(7.1,0.62,0.32));
#12694=CARTESIAN_POINT('',(7.1,0.712777777777778,0.32));
#12695=CARTESIAN_POINT('',(7.3,0.62,0.32));
#12696=CARTESIAN_POINT('',(10.,0.62,0.32));
#12697=CARTESIAN_POINT('',(7.3,-0.712777777777778,0.32));
#12698=CARTESIAN_POINT('Origin',(-0.0999999999999996,0.62,0.32));
#12699=CARTESIAN_POINT('',(7.1,0.62,0.));
#12700=CARTESIAN_POINT('',(7.1,0.62,0.16));
#12701=CARTESIAN_POINT('',(7.3,0.62,0.));
#12702=CARTESIAN_POINT('',(2.65,0.62,0.));
#12703=CARTESIAN_POINT('',(7.3,0.62,0.16));
#12704=CARTESIAN_POINT('Origin',(10.,1.30754691548544,0.));
#12705=CARTESIAN_POINT('',(10.,1.24211782565704,0.));
#12706=CARTESIAN_POINT('',(10.,-1.24211782565704,0.));
#12707=CARTESIAN_POINT('',(10.,1.30754691548544,0.));
#12708=CARTESIAN_POINT('',(10.,-1.20899340483173,0.605457329065657));
#12709=CARTESIAN_POINT('Ctrl Pts',(10.,-1.20899340483173,0.605457329065657));
#12710=CARTESIAN_POINT('Ctrl Pts',(10.,-1.21451837038612,0.504502771559899));
#12711=CARTESIAN_POINT('Ctrl Pts',(10.,-1.22004249263249,0.403547366186347));
#12712=CARTESIAN_POINT('Ctrl Pts',(10.,-1.23108392958594,0.201728789021226));
#12713=CARTESIAN_POINT('Ctrl Pts',(10.,-1.23660133320922,0.100864020914724));
#12714=CARTESIAN_POINT('Ctrl Pts',(10.,-1.24211782565704,0.));
#12715=CARTESIAN_POINT('Ctrl Pts',(10.,-1.10900986674273,0.7));
#12716=CARTESIAN_POINT('Ctrl Pts',(10.,-1.11692706738765,0.7));
#12717=CARTESIAN_POINT('Ctrl Pts',(9.99999896020971,-1.12478097169818,0.699006158364426));
#12718=CARTESIAN_POINT('Ctrl Pts',(9.99999805494427,-1.13243115645175,0.697118998397561));
#12719=CARTESIAN_POINT('Ctrl Pts',(9.99999754769332,-1.13671781459207,0.696061558623929));
#12720=CARTESIAN_POINT('Ctrl Pts',(9.99999708556116,-1.14094056283945,0.694722610426682));
#12721=CARTESIAN_POINT('Ctrl Pts',(9.99999679002998,-1.14507302265453,0.693112977943955));
#12722=CARTESIAN_POINT('Ctrl Pts',(9.99999625879002,-1.15250143622127,0.690219540062595));
#12723=CARTESIAN_POINT('Ctrl Pts',(9.999996365957,-1.15955821040664,0.686485807665162));
#12724=CARTESIAN_POINT('Ctrl Pts',(9.99999703387985,-1.16609707610076,0.681992895329386));
#12725=CARTESIAN_POINT('Ctrl Pts',(9.99999740034986,-1.16968476316425,0.679527763880215));
#12726=CARTESIAN_POINT('Ctrl Pts',(9.99999792190556,-1.17311627083768,0.676833210412541));
#12727=CARTESIAN_POINT('Ctrl Pts',(9.99999838578331,-1.17636354905877,0.673917165661822));
#12728=CARTESIAN_POINT('Ctrl Pts',(9.99999884023993,-1.17954487655573,0.671060344436104));
#12729=CARTESIAN_POINT('Ctrl Pts',(9.99999924462882,-1.18253006594632,0.668008218820746));
#12730=CARTESIAN_POINT('Ctrl Pts',(9.99999924442301,-1.185296421281,0.664772262763763));
#12731=CARTESIAN_POINT('Ctrl Pts',(9.99999924404215,-1.19041578560695,0.658783864313737));
#12732=CARTESIAN_POINT('Ctrl Pts',(9.99999800949836,-1.19478865237554,0.652167294255586));
#12733=CARTESIAN_POINT('Ctrl Pts',(9.99999759228052,-1.19835462180986,0.645087621913151));
#12734=CARTESIAN_POINT('Ctrl Pts',(9.99999755030119,-1.19871341999785,0.644375284453517));
#12735=CARTESIAN_POINT('Ctrl Pts',(9.9999975145836,-1.19906401030029,0.643658239626438));
#12736=CARTESIAN_POINT('Ctrl Pts',(9.99999748581823,-1.19940630408966,0.642936645100882));
#12737=CARTESIAN_POINT('Ctrl Pts',(9.99999720003888,-1.20280693749908,0.635767720253638));
#12738=CARTESIAN_POINT('Ctrl Pts',(9.9999978299417,-1.20535324884233,0.628234501710241));
#12739=CARTESIAN_POINT('Ctrl Pts',(9.99999874867777,-1.20699142055415,0.62050509267719));
#12740=CARTESIAN_POINT('Ctrl Pts',(9.99999933690345,-1.20804026874419,0.615556297251186));
#12741=CARTESIAN_POINT('Ctrl Pts',(9.99999999916487,-1.20871598809812,0.61052641213707));
#12742=CARTESIAN_POINT('Ctrl Pts',(9.99999999968202,-1.20899340489109,0.605457329065633));
#12743=CARTESIAN_POINT('Ctrl Pts',(10.,1.24211782565704,0.));
#12744=CARTESIAN_POINT('Ctrl Pts',(10.,1.23660053043673,0.100878698875723));
#12745=CARTESIAN_POINT('Ctrl Pts',(10.,1.23108232376984,0.201758145268796));
#12746=CARTESIAN_POINT('Ctrl Pts',(10.,1.22004088630648,0.403576722396156));
#12747=CARTESIAN_POINT('Ctrl Pts',(10.,1.2145175671044,0.504517449470448));
#12748=CARTESIAN_POINT('Ctrl Pts',(10.,1.20899340483173,0.605457329065657));
#12749=CARTESIAN_POINT('Origin',(7.3,-1.42555555555556,0.));
#12750=CARTESIAN_POINT('',(7.3,1.35236351479115,0.));
#12751=CARTESIAN_POINT('',(7.3,-1.42555555555556,0.));
#12752=CARTESIAN_POINT('Ctrl Pts',(7.29999999953133,1.3203161347307,0.605285370449834));
#12753=CARTESIAN_POINT('Ctrl Pts',(7.29999999953133,1.32565322760551,0.504490726585133));
#12754=CARTESIAN_POINT('Ctrl Pts',(7.3,1.33099015509697,0.403695123734478));
#12755=CARTESIAN_POINT('Ctrl Pts',(7.3,1.34167258064689,0.201933969199042));
#12756=CARTESIAN_POINT('Ctrl Pts',(7.3,1.34701817868136,0.100966514951419));
#12757=CARTESIAN_POINT('Ctrl Pts',(7.3,1.35236351479115,0.));
#12758=CARTESIAN_POINT('',(7.29999999953133,-1.3203161347307,0.605285370449834));
#12759=CARTESIAN_POINT('Ctrl Pts',(7.3,-1.32031613470337,0.605285370449877));
#12760=CARTESIAN_POINT('Ctrl Pts',(7.3,-1.31989712778929,0.61319860217968));
#12761=CARTESIAN_POINT('Ctrl Pts',(7.29999916171872,-1.31851071739963,0.621020829077898));
#12762=CARTESIAN_POINT('Ctrl Pts',(7.29999878808195,-1.31624092632926,0.628591660945423));
#12763=CARTESIAN_POINT('Ctrl Pts',(7.29999857947278,-1.31497365483497,0.632818613610392));
#12764=CARTESIAN_POINT('Ctrl Pts',(7.29999848639856,-1.31343001415,0.636967235874856));
#12765=CARTESIAN_POINT('Ctrl Pts',(7.29999853830689,-1.31161789606625,0.641007613679984));
#12766=CARTESIAN_POINT('Ctrl Pts',(7.29999863125487,-1.30837308502546,0.648242386418365));
#12767=CARTESIAN_POINT('Ctrl Pts',(7.29999925734287,-1.30430566789097,0.655052076019481));
#12768=CARTESIAN_POINT('Ctrl Pts',(7.29999949821933,-1.29947941328181,0.661273460789274));
#12769=CARTESIAN_POINT('Ctrl Pts',(7.29999954322,-1.29857776968225,0.662435743389828));
#12770=CARTESIAN_POINT('Ctrl Pts',(7.29999957102613,-1.29764951297213,0.663577423078133));
#12771=CARTESIAN_POINT('Ctrl Pts',(7.2999995707084,-1.29669488998092,0.664697318929248));
#12772=CARTESIAN_POINT('Ctrl Pts',(7.29999957007561,-1.29479368240016,0.666927680549918));
#12773=CARTESIAN_POINT('Ctrl Pts',(7.29999945886743,-1.29278792931167,0.669071688571899));
#12774=CARTESIAN_POINT('Ctrl Pts',(7.29999930790078,-1.2906849717248,0.671125563583336));
#12775=CARTESIAN_POINT('Ctrl Pts',(7.29999889984047,-1.28500071247856,0.676677153447665));
#12776=CARTESIAN_POINT('Ctrl Pts',(7.29999826931494,-1.27867319504519,0.681510485910933));
#12777=CARTESIAN_POINT('Ctrl Pts',(7.29999806345125,-1.27186607945067,0.685571085769401));
#12778=CARTESIAN_POINT('Ctrl Pts',(7.29999793266427,-1.26754145993833,0.688150820039508));
#12779=CARTESIAN_POINT('Ctrl Pts',(7.29999794545359,-1.26302231037287,0.690417984675215));
#12780=CARTESIAN_POINT('Ctrl Pts',(7.29999810371711,-1.25834494218995,0.69234933099425));
#12781=CARTESIAN_POINT('Ctrl Pts',(7.29999835129001,-1.25102809722258,0.695370551698293));
#12782=CARTESIAN_POINT('Ctrl Pts',(7.29999895574222,-1.24340909242398,0.6975375590939));
#12783=CARTESIAN_POINT('Ctrl Pts',(7.29999944081525,-1.2356348173965,0.698780605629559));
#12784=CARTESIAN_POINT('Ctrl Pts',(7.29999975409932,-1.23061380764338,0.699583426311495));
#12785=CARTESIAN_POINT('Ctrl Pts',(7.30000000047446,-1.22552743956586,0.699999999832051));
#12786=CARTESIAN_POINT('Ctrl Pts',(7.29999999989087,-1.22041345054982,0.7));
#12787=CARTESIAN_POINT('',(7.3,-1.35236351479115,0.));
#12788=CARTESIAN_POINT('Ctrl Pts',(7.3,-1.35236351479115,0.));
#12789=CARTESIAN_POINT('Ctrl Pts',(7.3,-1.34701814920095,0.100967071798286));
#12790=CARTESIAN_POINT('Ctrl Pts',(7.3,-1.34167252169398,0.201935082699409));
#12791=CARTESIAN_POINT('Ctrl Pts',(7.3,-1.33099009614589,0.403696237111114));
#12792=CARTESIAN_POINT('Ctrl Pts',(7.29999999953133,-1.32565319812959,0.504491283257837));
#12793=CARTESIAN_POINT('Ctrl Pts',(7.29999999953133,-1.3203161347307,0.605285370449834));
#12794=CARTESIAN_POINT('',(7.3,-1.42555555555556,0.));
#12795=CARTESIAN_POINT('Origin',(3.7,-1.44777777777778,0.));
#12796=CARTESIAN_POINT('',(3.7,1.37924639543935,0.));
#12797=CARTESIAN_POINT('',(3.7,-1.44777777777778,0.));
#12798=CARTESIAN_POINT('',(3.7,1.34735368793805,0.605261457205193));
#12799=CARTESIAN_POINT('Ctrl Pts',(3.7,1.34735368793805,0.605261457205193));
#12800=CARTESIAN_POINT('Ctrl Pts',(3.7,1.35266395147774,0.504488703431434));
#12801=CARTESIAN_POINT('Ctrl Pts',(3.7,1.35797406404029,0.40371594170176));
#12802=CARTESIAN_POINT('Ctrl Pts',(3.7,1.36860496587027,0.201962122597264));
#12803=CARTESIAN_POINT('Ctrl Pts',(3.7,1.37392575452088,0.100981065191366));
#12804=CARTESIAN_POINT('Ctrl Pts',(3.7,1.37924639543935,0.));
#12805=CARTESIAN_POINT('',(3.7,1.24747724070879,0.7));
#12806=CARTESIAN_POINT('Ctrl Pts',(3.7,1.24747724070879,0.7));
#12807=CARTESIAN_POINT('Ctrl Pts',(3.7,1.25538532734776,0.7));
#12808=CARTESIAN_POINT('Ctrl Pts',(3.70000034866643,1.26322972530331,0.699006048248363));
#12809=CARTESIAN_POINT('Ctrl Pts',(3.70000065268588,1.27087026624727,0.697119044026295));
#12810=CARTESIAN_POINT('Ctrl Pts',(3.7000008238479,1.27517186762995,0.696056666371322));
#12811=CARTESIAN_POINT('Ctrl Pts',(3.70000097972585,1.27940891103121,0.694710185093394));
#12812=CARTESIAN_POINT('Ctrl Pts',(3.70000107833511,1.28355469746902,0.693090631030141));
#12813=CARTESIAN_POINT('Ctrl Pts',(3.70000125487464,1.29097687270382,0.690191153635441));
#12814=CARTESIAN_POINT('Ctrl Pts',(3.7000012145424,1.29802606517866,0.686451118058958));
#12815=CARTESIAN_POINT('Ctrl Pts',(3.70000098691147,1.3045562506385,0.681952404110064));
#12816=CARTESIAN_POINT('Ctrl Pts',(3.70000086156653,1.30815209635338,0.679475187900035));
#12817=CARTESIAN_POINT('Ctrl Pts',(3.70000068390876,1.31159030769532,0.676767042898431));
#12818=CARTESIAN_POINT('Ctrl Pts',(3.70000052608992,1.31484259178137,0.673836088143417));
#12819=CARTESIAN_POINT('Ctrl Pts',(3.70000037216713,1.31801458722906,0.670977489418868));
#12820=CARTESIAN_POINT('Ctrl Pts',(3.70000023558528,1.32099045552882,0.667924239810466));
#12821=CARTESIAN_POINT('Ctrl Pts',(3.70000023595245,1.32374763345498,0.664687876924229));
#12822=CARTESIAN_POINT('Ctrl Pts',(3.70000023663259,1.32885491153898,0.658692977181302));
#12823=CARTESIAN_POINT('Ctrl Pts',(3.70000065621025,1.33321474659758,0.652071180203097));
#12824=CARTESIAN_POINT('Ctrl Pts',(3.70000080093706,1.33676785491319,0.644988218508662));
#12825=CARTESIAN_POINT('Ctrl Pts',(3.70000081573428,1.33713113341147,0.644264039153811));
#12826=CARTESIAN_POINT('Ctrl Pts',(3.70000082835625,1.33748593861467,0.643535019157411));
#12827=CARTESIAN_POINT('Ctrl Pts',(3.70000083855542,1.33783217873901,0.642801324492746));
#12828=CARTESIAN_POINT('Ctrl Pts',(3.70000093832019,1.34121897990539,0.63562457699476));
#12829=CARTESIAN_POINT('Ctrl Pts',(3.70000072997693,1.34375116782692,0.628085030530103));
#12830=CARTESIAN_POINT('Ctrl Pts',(3.70000042189378,1.34537558692779,0.6203512574804));
#12831=CARTESIAN_POINT('Ctrl Pts',(3.70000022417294,1.3464181026242,0.615387895628485));
#12832=CARTESIAN_POINT('Ctrl Pts',(3.70000000036652,1.34708586836718,0.6103438638189));
#12833=CARTESIAN_POINT('Ctrl Pts',(3.69999999992214,1.34735368792773,0.6052614572053));
#12834=CARTESIAN_POINT('',(3.7,-1.24747724070944,0.7));
#12835=CARTESIAN_POINT('',(3.7,-0.723888888888889,0.7));
#12836=CARTESIAN_POINT('',(3.7,-1.34735368793805,0.605261457205193));
#12837=CARTESIAN_POINT('Ctrl Pts',(3.69999999992215,-1.34735368792773,0.6052614572053));
#12838=CARTESIAN_POINT('Ctrl Pts',(3.70000000061408,-1.34693666923469,0.613175212866596));
#12839=CARTESIAN_POINT('Ctrl Pts',(3.70000049671034,-1.34555248374866,0.620998392122869));
#12840=CARTESIAN_POINT('Ctrl Pts',(3.70000071566022,-1.34328499565267,0.628570462735333));
#12841=CARTESIAN_POINT('Ctrl Pts',(3.70000083807517,-1.34201724238155,0.632804009674372));
#12842=CARTESIAN_POINT('Ctrl Pts',(3.7000008913247,-1.34047237297042,0.63695909738719));
#12843=CARTESIAN_POINT('Ctrl Pts',(3.70000085837557,-1.33865827982058,0.641005656934072));
#12844=CARTESIAN_POINT('Ctrl Pts',(3.7000007994669,-1.33541492172585,0.648240369034365));
#12845=CARTESIAN_POINT('Ctrl Pts',(3.70000042420685,-1.33134915897915,0.655050234746405));
#12846=CARTESIAN_POINT('Ctrl Pts',(3.70000027984635,-1.32652447879733,0.661271863919233));
#12847=CARTESIAN_POINT('Ctrl Pts',(3.70000025294096,-1.32562527203035,0.662431429080655));
#12848=CARTESIAN_POINT('Ctrl Pts',(3.7000002362737,-1.32469957579387,0.663570491348455));
#12849=CARTESIAN_POINT('Ctrl Pts',(3.70000023630138,-1.32374763346102,0.664687876924223));
#12850=CARTESIAN_POINT('Ctrl Pts',(3.70000023635686,-1.32184039796576,0.666926581264246));
#12851=CARTESIAN_POINT('Ctrl Pts',(3.70000030283857,-1.31982784222224,0.669078323867587));
#12852=CARTESIAN_POINT('Ctrl Pts',(3.70000039320883,-1.31771738411303,0.671139279696989));
#12853=CARTESIAN_POINT('Ctrl Pts',(3.70000063660146,-1.3120333248939,0.676690015307994));
#12854=CARTESIAN_POINT('Ctrl Pts',(3.7000010126336,-1.30570602994251,0.681522474044465));
#12855=CARTESIAN_POINT('Ctrl Pts',(3.70000113724274,-1.29889910811053,0.685582059356066));
#12856=CARTESIAN_POINT('Ctrl Pts',(3.70000121634872,-1.29457784995583,0.688159217808216));
#12857=CARTESIAN_POINT('Ctrl Pts',(3.70000121058612,-1.2900623422215,0.690424215862126));
#12858=CARTESIAN_POINT('Ctrl Pts',(3.70000111831253,-1.28538881676413,0.692353818784707));
#12859=CARTESIAN_POINT('Ctrl Pts',(3.70000097388434,-1.27807373536961,0.695374066040565));
#12860=CARTESIAN_POINT('Ctrl Pts',(3.70000061691996,-1.27045659963863,0.697540160564298));
#12861=CARTESIAN_POINT('Ctrl Pts',(3.7000003304055,-1.26268427129293,0.698782316368755));
#12862=CARTESIAN_POINT('Ctrl Pts',(3.70000014548661,-1.25766794365683,0.699584014420239));
#12863=CARTESIAN_POINT('Ctrl Pts',(3.7,-1.25258637988459,0.7));
#12864=CARTESIAN_POINT('Ctrl Pts',(3.7,-1.24747724070879,0.7));
#12865=CARTESIAN_POINT('',(3.7,-1.37924639543935,0.));
#12866=CARTESIAN_POINT('Ctrl Pts',(3.7,-1.37924639543935,0.));
#12867=CARTESIAN_POINT('Ctrl Pts',(3.7,-1.37392574223662,0.100981298335747));
#12868=CARTESIAN_POINT('Ctrl Pts',(3.7,-1.36860494130098,0.201962588887634));
#12869=CARTESIAN_POINT('Ctrl Pts',(3.7,-1.35797403946962,0.403716407992068));
#12870=CARTESIAN_POINT('Ctrl Pts',(3.7,-1.3526639391921,0.504488936575732));
#12871=CARTESIAN_POINT('Ctrl Pts',(3.7,-1.34735368793805,0.605261457205193));
#12872=CARTESIAN_POINT('',(3.7,-1.44777777777778,0.));
#12873=CARTESIAN_POINT('Origin',(1.1,-1.34328341716202,0.));
#12874=CARTESIAN_POINT('',(1.1,1.27885335043294,0.));
#12875=CARTESIAN_POINT('',(1.1,-1.34328341716202,0.));
#12876=CARTESIAN_POINT('Ctrl Pts',(1.1,1.24553911298206,0.605485603995113));
#12877=CARTESIAN_POINT('Ctrl Pts',(1.1,1.25109559382646,0.504544105903265));
#12878=CARTESIAN_POINT('Ctrl Pts',(1.1,1.25665083308595,0.403601248768354));
#12879=CARTESIAN_POINT('Ctrl Pts',(1.1,1.26775551906787,0.201773573764085));
#12880=CARTESIAN_POINT('Ctrl Pts',(1.1,1.2733051088238,0.100886182270816));
#12881=CARTESIAN_POINT('Ctrl Pts',(1.1,1.27885335043294,0.));
#12882=CARTESIAN_POINT('',(1.1,-1.14549341399195,0.7));
#12883=CARTESIAN_POINT('',(1.1,-0.671641708581009,0.7));
#12884=CARTESIAN_POINT('',(1.1,-1.24553911298206,0.605485603995113));
#12885=CARTESIAN_POINT('Ctrl Pts',(1.09999999916631,-1.24553911263843,0.605485603997431));
#12886=CARTESIAN_POINT('Ctrl Pts',(1.10000000220634,-1.24510362317222,0.61339691285734));
#12887=CARTESIAN_POINT('Ctrl Pts',(1.10000177015643,-1.24370036622144,0.621215229994996));
#12888=CARTESIAN_POINT('Ctrl Pts',(1.10000252895322,-1.24141353486351,0.628780213666851));
#12889=CARTESIAN_POINT('Ctrl Pts',(1.10000294802756,-1.24015054543059,0.632958263090869));
#12890=CARTESIAN_POINT('Ctrl Pts',(1.10000312162076,-1.23861706177488,0.637059070655947));
#12891=CARTESIAN_POINT('Ctrl Pts',(1.10000299297862,-1.23682078380192,0.641053713130525));
#12892=CARTESIAN_POINT('Ctrl Pts',(1.10000275999609,-1.23356756237267,0.64828837095969));
#12893=CARTESIAN_POINT('Ctrl Pts',(1.10000138715103,-1.22949085733774,0.655096441442141));
#12894=CARTESIAN_POINT('Ctrl Pts',(1.10000084482056,-1.2246552743941,0.661315040399663));
#12895=CARTESIAN_POINT('Ctrl Pts',(1.10000074196669,-1.22373819809959,0.662494407966206));
#12896=CARTESIAN_POINT('Ctrl Pts',(1.1000006773267,-1.22279369438101,0.663652502541609));
#12897=CARTESIAN_POINT('Ctrl Pts',(1.10000067553493,-1.22182202641035,0.66478809188211));
#12898=CARTESIAN_POINT('Ctrl Pts',(1.10000067210542,-1.219962222636,0.666961646435043));
#12899=CARTESIAN_POINT('Ctrl Pts',(1.10000089707048,-1.21800293160495,0.669052796220007));
#12900=CARTESIAN_POINT('Ctrl Pts',(1.10000120920309,-1.21595100691259,0.671058078730413));
#12901=CARTESIAN_POINT('Ctrl Pts',(1.10000207391986,-1.21026645613745,0.676613414309409));
#12902=CARTESIAN_POINT('Ctrl Pts',(1.1000034579227,-1.20393786500476,0.681450029097565));
#12903=CARTESIAN_POINT('Ctrl Pts',(1.10000394126019,-1.19712964857754,0.685514663758263));
#12904=CARTESIAN_POINT('Ctrl Pts',(1.10000424974863,-1.19278432848208,0.688108902478585));
#12905=CARTESIAN_POINT('Ctrl Pts',(1.10000425197701,-1.18824265871575,0.690387991283085));
#12906=CARTESIAN_POINT('Ctrl Pts',(1.10000394032285,-1.18354156621637,0.692328715646671));
#12907=CARTESIAN_POINT('Ctrl Pts',(1.10000345443802,-1.17621232165581,0.695354404566264));
#12908=CARTESIAN_POINT('Ctrl Pts',(1.10000219938511,-1.16858027633095,0.697525330589554));
#12909=CARTESIAN_POINT('Ctrl Pts',(1.10000118192936,-1.16079305972554,0.698772417158578));
#12910=CARTESIAN_POINT('Ctrl Pts',(1.10000052251962,-1.15574619011492,0.699580649884844));
#12911=CARTESIAN_POINT('Ctrl Pts',(1.1,-1.15063354328712,0.7));
#12912=CARTESIAN_POINT('Ctrl Pts',(1.1,-1.14549341399196,0.7));
#12913=CARTESIAN_POINT('',(1.1,-1.27885335043294,0.));
#12914=CARTESIAN_POINT('Ctrl Pts',(1.1,-1.27885335043294,0.));
#12915=CARTESIAN_POINT('Ctrl Pts',(1.1,-1.27330503870861,0.100887457206881));
#12916=CARTESIAN_POINT('Ctrl Pts',(1.1,-1.26775537880223,0.201776123688554));
#12917=CARTESIAN_POINT('Ctrl Pts',(1.1,-1.25665069275548,0.403603798678134));
#12918=CARTESIAN_POINT('Ctrl Pts',(1.1,-1.25109552364596,0.504545380833391));
#12919=CARTESIAN_POINT('Ctrl Pts',(1.1,-1.24553911298206,0.605485603995113));
#12920=CARTESIAN_POINT('',(1.1,-1.34328341716202,0.));
#12921=CARTESIAN_POINT('Origin',(0.199725906950915,-1.4,-0.0104671912485888));
#12922=CARTESIAN_POINT('',(0.200274469199584,1.12301388185427,1.38777878078145E-17));
#12923=CARTESIAN_POINT('',(0.200274469199585,-0.7,0.));
#12924=CARTESIAN_POINT('',(0.231993417893744,1.09142177001972,0.605233595624295));
#12925=CARTESIAN_POINT('Ctrl Pts',(0.200274469199584,1.12301388185427,-2.97071395261028E-17));
#12926=CARTESIAN_POINT('Ctrl Pts',(0.210847451470635,1.11248294808,0.201744519910852));
#12927=CARTESIAN_POINT('Ctrl Pts',(0.22142043436526,1.101952242875,0.403489051720196));
#12928=CARTESIAN_POINT('Ctrl Pts',(0.231993417893744,1.09142177001972,0.605233595624295));
#12929=CARTESIAN_POINT('',(0.231993417893744,-1.09142177001972,0.605233595624295));
#12930=CARTESIAN_POINT('',(0.231993417893744,-0.7,0.605233595624295));
#12931=CARTESIAN_POINT('',(0.200274469199584,-1.12301388185427,-1.38777878078145E-17));
#12932=CARTESIAN_POINT('Ctrl Pts',(0.231993417893744,-1.09142177001972,
0.605233595624295));
#12933=CARTESIAN_POINT('Ctrl Pts',(0.22142043436526,-1.101952242875,0.403489051720196));
#12934=CARTESIAN_POINT('Ctrl Pts',(0.210847451470635,-1.11248294808,0.201744519910852));
#12935=CARTESIAN_POINT('Ctrl Pts',(0.200274469199584,-1.12301388185427,
-4.90059381963448E-17));
#12936=CARTESIAN_POINT('',(0.200274469199585,-0.7,0.));
#12937=CARTESIAN_POINT('Origin',(5.4,-1.11022302462516E-16,0.));
#12938=CARTESIAN_POINT('Ctrl Pts',(7.29999999999999,-1.35236351479115,1.04083408558608E-17));
#12939=CARTESIAN_POINT('Ctrl Pts',(8.20044803681595,-1.32637404707459,3.18306896032855E-8));
#12940=CARTESIAN_POINT('Ctrl Pts',(9.10060048441536,-1.28803709316692,1.03188250195688E-8));
#12941=CARTESIAN_POINT('Ctrl Pts',(10.0000000000405,-1.24211782537639,-8.23328475353175E-12));
#12942=CARTESIAN_POINT('Ctrl Pts',(10.0000000000405,1.24211782537639,-8.23320567538283E-12));
#12943=CARTESIAN_POINT('Ctrl Pts',(9.1006004808701,1.28803709334794,1.03184817085883E-8));
#12944=CARTESIAN_POINT('Ctrl Pts',(8.20044803144508,1.32637404722969,3.18291413954212E-8));
#12945=CARTESIAN_POINT('Ctrl Pts',(7.3,1.35236351479115,4.75121773919879E-17));
#12946=CARTESIAN_POINT('',(7.1,1.35793097395724,0.));
#12947=CARTESIAN_POINT('',(7.1,1.42555555555556,0.));
#12948=CARTESIAN_POINT('Ctrl Pts',(7.1000000000396,1.35793097389613,-4.88924676637329E-12));
#12949=CARTESIAN_POINT('Ctrl Pts',(6.53177385320612,1.37316067096195,3.71763852401782E-9));
#12950=CARTESIAN_POINT('Ctrl Pts',(5.96344379069665,1.38333257666104,-3.82408184804385E-8));
#12951=CARTESIAN_POINT('Ctrl Pts',(5.39512359652123,1.38725406840392,-3.97623797275691E-8));
#12952=CARTESIAN_POINT('Ctrl Pts',(4.82973248928002,1.39115534902226,-4.12760989429076E-8));
#12953=CARTESIAN_POINT('Ctrl Pts',(4.26470859812609,1.38886839226708,1.63957607983357E-8));
#12954=CARTESIAN_POINT('Ctrl Pts',(3.70000000036239,1.37924639538501,-6.25376529969227E-12));
#12955=CARTESIAN_POINT('',(3.5,1.37552980833516,0.));
#12956=CARTESIAN_POINT('',(3.5,1.44777777777778,0.));
#12957=CARTESIAN_POINT('Ctrl Pts',(3.50000000097466,1.37552980835479,1.06251812903579E-15));
#12958=CARTESIAN_POINT('Ctrl Pts',(2.69943075695685,1.35940904975719,2.35366119539541E-7));
#12959=CARTESIAN_POINT('Ctrl Pts',(1.89948254587541,1.32827224396921,2.51300192353997E-7));
#12960=CARTESIAN_POINT('Ctrl Pts',(1.10000000028363,1.27885335028943,-5.13283415455519E-11));
#12961=CARTESIAN_POINT('',(0.9,1.266106713614,0.));
#12962=CARTESIAN_POINT('',(0.9,1.34328341716202,0.));
#12963=CARTESIAN_POINT('',(0.292382661757373,1.22257596919059,0.));
#12964=CARTESIAN_POINT('Ctrl Pts',(0.9,1.266106713614,1.20346441145891E-16));
#12965=CARTESIAN_POINT('Ctrl Pts',(0.697432754539207,1.25280566772398,-2.10387859372414E-8));
#12966=CARTESIAN_POINT('Ctrl Pts',(0.494894520889663,1.23831317328004,3.6654767345328E-12));
#12967=CARTESIAN_POINT('Ctrl Pts',(0.292382661757371,1.22257596919059,2.98331735103528E-16));
#12968=CARTESIAN_POINT('Ctrl Pts',(0.292382661757373,1.22257596919059,2.94902990916057E-17));
#12969=CARTESIAN_POINT('Ctrl Pts',(0.284469747869226,1.22196105627757,-8.65621238729993E-13));
#12970=CARTESIAN_POINT('Ctrl Pts',(0.276673396002317,1.22038240716686,-1.19564355630166E-6));
#12971=CARTESIAN_POINT('Ctrl Pts',(0.269153172408756,1.21792571627104,-1.29137975931779E-6));
#12972=CARTESIAN_POINT('Ctrl Pts',(0.264330998492885,1.21635041859408,-1.35276844214688E-6));
#12973=CARTESIAN_POINT('Ctrl Pts',(0.259622238853914,1.21441292414196,-1.0165784587106E-6));
#12974=CARTESIAN_POINT('Ctrl Pts',(0.255072584042237,1.21212521597766,-4.21167369976509E-7));
#12975=CARTESIAN_POINT('Ctrl Pts',(0.247984787860257,1.20856125126747,5.06409032217246E-7));
#12976=CARTESIAN_POINT('Ctrl Pts',(0.241364979299678,1.20419126978451,2.25366520907849E-6));
#12977=CARTESIAN_POINT('Ctrl Pts',(0.235375785094684,1.19908071490398,1.28723124315333E-6));
#12978=CARTESIAN_POINT('Ctrl Pts',(0.235058634311792,1.19881009144014,1.23605486142058E-6));
#12979=CARTESIAN_POINT('Ctrl Pts',(0.234743258170683,1.19853738091759,1.17639378419006E-6));
#12980=CARTESIAN_POINT('Ctrl Pts',(0.234429683218046,1.19826258967301,1.10742116603597E-6));
#12981=CARTESIAN_POINT('Ctrl Pts',(0.23095881299434,1.19522100506769,3.4398325561458E-7));
#12982=CARTESIAN_POINT('Ctrl Pts',(0.227708211416394,1.19192479473749,-1.52348441667556E-6));
#12983=CARTESIAN_POINT('Ctrl Pts',(0.224692430858345,1.18840300965977,-3.42436181452249E-6));
#12984=CARTESIAN_POINT('Ctrl Pts',(0.219522873151367,1.18236607466387,-6.68278702580898E-6));
#12985=CARTESIAN_POINT('Ctrl Pts',(0.21509942609515,1.17573654654733,-9.78259773483875E-6));
#12986=CARTESIAN_POINT('Ctrl Pts',(0.211478909386775,1.16867548752938,-1.04320859863301E-5));
#12987=CARTESIAN_POINT('Ctrl Pts',(0.20968494559888,1.16517673715679,-1.075390701291E-5));
#12988=CARTESIAN_POINT('Ctrl Pts',(0.208088728862602,1.16157146972622,-1.05358292927083E-5));
#12989=CARTESIAN_POINT('Ctrl Pts',(0.206701335101202,1.15787708229469,-9.83193564179307E-6));
#12990=CARTESIAN_POINT('Ctrl Pts',(0.203919119965097,1.15046852899383,-8.42037994342582E-6));
#12991=CARTESIAN_POINT('Ctrl Pts',(0.202003457218558,1.1427818296106,-4.88542801801716E-6));
#12992=CARTESIAN_POINT('Ctrl Pts',(0.201024541128784,1.13496408391561,-2.30807221316776E-6));
#12993=CARTESIAN_POINT('Ctrl Pts',(0.200529226009753,1.13100843574523,-1.00397341389412E-6));
#12994=CARTESIAN_POINT('Ctrl Pts',(0.200274469344113,1.12701892049093,-1.14168925800036E-11));
#12995=CARTESIAN_POINT('Ctrl Pts',(0.200274469199584,1.12301388185427,-1.43114686768087E-17));
#12996=CARTESIAN_POINT('',(-1.73234772679968E-18,1.12356026268968,4.53319947845445E-20));
#12997=CARTESIAN_POINT('',(0.,-1.4,0.));
#12998=CARTESIAN_POINT('',(0.276326924564679,1.42224670711126,-2.77555756156289E-17));
#12999=CARTESIAN_POINT('Ctrl Pts',(0.276326924564681,1.42224670711126,-1.50920942409982E-16));
#13000=CARTESIAN_POINT('Ctrl Pts',(0.258529852003869,1.4208638358667,-3.32972379743633E-13));
#13001=CARTESIAN_POINT('Ctrl Pts',(0.240927013527826,1.41785398988725,-1.99727536601662E-6));
#13002=CARTESIAN_POINT('Ctrl Pts',(0.223720619657732,1.41333325652174,-2.71091968639774E-6));
#13003=CARTESIAN_POINT('Ctrl Pts',(0.206313289378911,1.40875972999491,-3.432897951005E-6));
#13004=CARTESIAN_POINT('Ctrl Pts',(0.18931019325249,1.40263932318529,-2.78724979559428E-6));
#13005=CARTESIAN_POINT('Ctrl Pts',(0.172932985028856,1.39504220432096,-6.31841720307455E-7));
#13006=CARTESIAN_POINT('Ctrl Pts',(0.170060146426803,1.39370954151055,-2.53746782677961E-7));
#13007=CARTESIAN_POINT('Ctrl Pts',(0.167206630967902,1.39233132643846,1.61597591574489E-7));
#13008=CARTESIAN_POINT('Ctrl Pts',(0.164373729059928,1.39090779908693,6.02790108062464E-7));
#13009=CARTESIAN_POINT('Ctrl Pts',(0.148213121449433,1.38278712717586,3.11962244863226E-6));
#13010=CARTESIAN_POINT('Ctrl Pts',(0.132864864406694,1.37326763401578,6.8005293729143E-6));
#13011=CARTESIAN_POINT('Ctrl Pts',(0.118540368157823,1.36244192017091,7.47011412280372E-6));
#13012=CARTESIAN_POINT('Ctrl Pts',(0.1130124780146,1.35826422653222,7.72851001154276E-6));
#13013=CARTESIAN_POINT('Ctrl Pts',(0.107637267132642,1.35389150739715,7.50091387420595E-6));
#13014=CARTESIAN_POINT('Ctrl Pts',(0.102427993107927,1.34932731552598,6.39696583889361E-6));
#13015=CARTESIAN_POINT('Ctrl Pts',(0.0920147884934566,1.34020361352282,
4.19020214765608E-6));
#13016=CARTESIAN_POINT('Ctrl Pts',(0.082263696775192,1.33031540618347,-1.43705507633734E-6));
#13017=CARTESIAN_POINT('Ctrl Pts',(0.0732179607829324,1.31975004019149,
-7.24116446069057E-6));
#13018=CARTESIAN_POINT('Ctrl Pts',(0.0614369648181435,1.30598990677343,
-1.48003270644599E-5));
#13019=CARTESIAN_POINT('Ctrl Pts',(0.0509520748529884,1.29120077200215,
-2.24515165560165E-5));
#13020=CARTESIAN_POINT('Ctrl Pts',(0.0418305631051555,1.27560026299671,
-2.64881615939377E-5));
#13021=CARTESIAN_POINT('Ctrl Pts',(0.0329966685655992,1.26049166530727,
-3.03975241584371E-5));
#13022=CARTESIAN_POINT('Ctrl Pts',(0.0254411283904758,1.24462062939249,
-3.09701348507133E-5));
#13023=CARTESIAN_POINT('Ctrl Pts',(0.0192647836588538,1.2281607987719,-2.81763116144976E-5));
#13024=CARTESIAN_POINT('Ctrl Pts',(0.0129258683931997,1.2112677210496,-2.53089508159798E-5));
#13025=CARTESIAN_POINT('Ctrl Pts',(0.00809110271874438,1.19389182855556,
-1.89493195503086E-5));
#13026=CARTESIAN_POINT('Ctrl Pts',(0.00484442764459327,1.17622983835018,
-1.25518552566888E-5));
#13027=CARTESIAN_POINT('Ctrl Pts',(0.00165723550742335,1.1588914367474,
-6.27160009448058E-6));
#13028=CARTESIAN_POINT('Ctrl Pts',(1.90718451428807E-9,1.14127598190669,
-1.51296892603399E-10));
#13029=CARTESIAN_POINT('Ctrl Pts',(2.41777084464267E-17,1.12356026268968,
-3.46944695195361E-18));
#13030=CARTESIAN_POINT('',(10.5166159648474,1.4155315881283,0.));
#13031=CARTESIAN_POINT('Ctrl Pts',(0.276326924564679,1.42224670711126,0.));
#13032=CARTESIAN_POINT('Ctrl Pts',(3.68975660465893,1.68747752195839,0.));
#13033=CARTESIAN_POINT('Ctrl Pts',(7.10318628475318,1.599994843061,0.));
#13034=CARTESIAN_POINT('Ctrl Pts',(10.5166159648474,1.4155315881283,0.));
#13035=CARTESIAN_POINT('',(10.8,1.11638029377732,-5.56631991785941E-17));
#13036=CARTESIAN_POINT('Ctrl Pts',(10.8,1.11638029377732,2.32452945780892E-16));
#13037=CARTESIAN_POINT('Ctrl Pts',(10.7999999994302,1.13421844616111,-9.29296349749781E-12));
#13038=CARTESIAN_POINT('Ctrl Pts',(10.7983603663884,1.15198349698667,-2.38856955364628E-6));
#13039=CARTESIAN_POINT('Ctrl Pts',(10.7951843826221,1.16946861094468,-3.77014304120448E-6));
#13040=CARTESIAN_POINT('Ctrl Pts',(10.7919669771209,1.18718176881198,-5.16973525142236E-6));
#13041=CARTESIAN_POINT('Ctrl Pts',(10.7871724978816,1.20460918321158,-5.4755482503851E-6));
#13042=CARTESIAN_POINT('Ctrl Pts',(10.7808573412527,1.22152732075962,-4.27334038376583E-6));
#13043=CARTESIAN_POINT('Ctrl Pts',(10.7797421066656,1.22451500471617,-4.06103467663179E-6));
#13044=CARTESIAN_POINT('Ctrl Pts',(10.7785793293545,1.22748675045939,-3.81081650224554E-6));
#13045=CARTESIAN_POINT('Ctrl Pts',(10.7773691713543,1.23044124224994,-3.53261416912234E-6));
#13046=CARTESIAN_POINT('Ctrl Pts',(10.7705159051166,1.24717287467681,-1.95712183132163E-6));
#13047=CARTESIAN_POINT('Ctrl Pts',(10.7622076549587,1.26320448426569,8.50150473021234E-7));
#13048=CARTESIAN_POINT('Ctrl Pts',(10.7525236566209,1.27832128496499,1.09915986206012E-6));
#13049=CARTESIAN_POINT('Ctrl Pts',(10.7482509716548,1.28499098118248,1.20902550183604E-6));
#13050=CARTESIAN_POINT('Ctrl Pts',(10.7437098328292,1.29148238441373,7.76315258636623E-7));
#13051=CARTESIAN_POINT('Ctrl Pts',(10.7389041877712,1.29777551763099,-7.54184826032082E-7));
#13052=CARTESIAN_POINT('Ctrl Pts',(10.7310976851069,1.30799836193882,-3.24039694621926E-6));
#13053=CARTESIAN_POINT('Ctrl Pts',(10.7225935645301,1.31769858917671,-8.57388820182801E-6));
#13054=CARTESIAN_POINT('Ctrl Pts',(10.7134588931078,1.3268364513864,-1.41086939541967E-5));
#13055=CARTESIAN_POINT('Ctrl Pts',(10.7004433550849,1.33985653580309,-2.19949628070403E-5));
#13056=CARTESIAN_POINT('Ctrl Pts',(10.6862650266646,1.35162127070648,-3.0022236679635E-5));
#13057=CARTESIAN_POINT('Ctrl Pts',(10.6711476119081,1.36204513612776,-3.40981369893719E-5));
#13058=CARTESIAN_POINT('Ctrl Pts',(10.6560301971515,1.37246900154903,-3.81740372991087E-5));
#13059=CARTESIAN_POINT('Ctrl Pts',(10.6399721826852,1.38155285075117,-3.83332859284948E-5));
#13060=CARTESIAN_POINT('Ctrl Pts',(10.6231652498763,1.38916602817047,-3.45204725343976E-5));
#13061=CARTESIAN_POINT('Ctrl Pts',(10.6063487480974,1.39678354012646,-3.07054883279539E-5));
#13062=CARTESIAN_POINT('Ctrl Pts',(10.5889271210941,1.40286310406803,-2.29928881382306E-5));
#13063=CARTESIAN_POINT('Ctrl Pts',(10.5711041279812,1.40730078588308,-1.53078138731408E-5));
#13064=CARTESIAN_POINT('Ctrl Pts',(10.5532811348684,1.41173846769814,-7.6227396080509E-6));
#13065=CARTESIAN_POINT('Ctrl Pts',(10.5350552605908,1.41453511891929,-9.16729947674095E-11));
#13066=CARTESIAN_POINT('Ctrl Pts',(10.5166159648474,1.4155315881283,2.48932818802672E-16));
#13067=CARTESIAN_POINT('',(10.8,-1.11638029377732,-1.39157997946485E-17));
#13068=CARTESIAN_POINT('',(10.8,1.4,0.));
#13069=CARTESIAN_POINT('',(10.5166159648474,-1.4155315881283,2.77555756156289E-17));
#13070=CARTESIAN_POINT('Ctrl Pts',(10.5166159648474,-1.4155315881283,-1.94289029309402E-16));
#13071=CARTESIAN_POINT('Ctrl Pts',(10.5344251606169,-1.41456917089032,1.72780596414851E-12));
#13072=CARTESIAN_POINT('Ctrl Pts',(10.5520727686739,-1.41197333457428,-2.53403886306205E-6));
#13073=CARTESIAN_POINT('Ctrl Pts',(10.5693578805681,-1.40785843881911,-4.04156906196095E-6));
#13074=CARTESIAN_POINT('Ctrl Pts',(10.5868701251756,-1.40368947182374,-5.56890876087065E-6));
#13075=CARTESIAN_POINT('Ctrl Pts',(10.604011804524,-1.39796079212135,-5.98742339745246E-6));
#13076=CARTESIAN_POINT('Ctrl Pts',(10.6205627760847,-1.39074087128671,-4.81856832951796E-6));
#13077=CARTESIAN_POINT('Ctrl Pts',(10.6234754753687,-1.38947028374636,-4.61286902618664E-6));
#13078=CARTESIAN_POINT('Ctrl Pts',(10.6263698187278,-1.38815339768352,-4.36721670635639E-6));
#13079=CARTESIAN_POINT('Ctrl Pts',(10.629244514885,-1.38679044403738,-4.09122931699412E-6));
#13080=CARTESIAN_POINT('Ctrl Pts',(10.6455827855986,-1.37904412775797,-2.5226612199239E-6));
#13081=CARTESIAN_POINT('Ctrl Pts',(10.6611432679573,-1.36988219838444,3.58605122725343E-7));
#13082=CARTESIAN_POINT('Ctrl Pts',(10.6757157985124,-1.35939560704671,7.40589063327193E-7));
#13083=CARTESIAN_POINT('Ctrl Pts',(10.6821516119741,-1.35476430808026,9.09288478831296E-7));
#13084=CARTESIAN_POINT('Ctrl Pts',(10.6883944859408,-1.34987400891586,5.44816430868337E-7));
#13085=CARTESIAN_POINT('Ctrl Pts',(10.6944246343503,-1.34472976213865,-9.14752338109426E-7));
#13086=CARTESIAN_POINT('Ctrl Pts',(10.7041966733629,-1.33639335368171,-3.28002794718031E-6));
#13087=CARTESIAN_POINT('Ctrl Pts',(10.7134106653983,-1.3273903805878,-8.47259327327479E-6));
#13088=CARTESIAN_POINT('Ctrl Pts',(10.7220307555455,-1.31778973409553,-1.38734771921913E-5));
#13089=CARTESIAN_POINT('Ctrl Pts',(10.7343338492722,-1.3040871333553,-2.15819326638919E-5));
#13090=CARTESIAN_POINT('Ctrl Pts',(10.7453199276401,-1.28929041974124,-2.94555326738194E-5));
#13091=CARTESIAN_POINT('Ctrl Pts',(10.7549158277293,-1.27362793268665,-3.3443536645081E-5));
#13092=CARTESIAN_POINT('Ctrl Pts',(10.7645117278185,-1.25796544563206,-3.74315406163426E-5));
#13093=CARTESIAN_POINT('Ctrl Pts',(10.7727182208071,-1.24143562566754,-3.75750290962259E-5));
#13094=CARTESIAN_POINT('Ctrl Pts',(10.7794153247677,-1.22423716044977,-3.38265125308188E-5));
#13095=CARTESIAN_POINT('Ctrl Pts',(10.7861166764432,-1.20702778690835,-3.00756184258222E-5));
#13096=CARTESIAN_POINT('Ctrl Pts',(10.7912490477072,-1.18929683429644,-2.25107044755726E-5));
#13097=CARTESIAN_POINT('Ctrl Pts',(10.7947196858669,-1.17125359626911,-1.49815203503087E-5));
#13098=CARTESIAN_POINT('Ctrl Pts',(10.7981903240266,-1.15321035824179,-7.45233622504479E-6));
#13099=CARTESIAN_POINT('Ctrl Pts',(10.7999999985278,-1.13485327409571,-1.17780195603766E-10));
#13100=CARTESIAN_POINT('Ctrl Pts',(10.8,-1.11638029377732,-1.38777878078145E-17));
#13101=CARTESIAN_POINT('',(0.276326924564679,-1.42224670711126,-5.55111512312578E-17));
#13102=CARTESIAN_POINT('Ctrl Pts',(10.5166159648474,-1.4155315881283,0.));
#13103=CARTESIAN_POINT('Ctrl Pts',(7.10318628475318,-1.599994843061,0.));
#13104=CARTESIAN_POINT('Ctrl Pts',(3.68975660465893,-1.68747752195839,0.));
#13105=CARTESIAN_POINT('Ctrl Pts',(0.276326924564679,-1.42224670711126,
0.));
#13106=CARTESIAN_POINT('',(-7.25311916552711E-19,-1.12356026268968,1.39157997946485E-17));
#13107=CARTESIAN_POINT('Ctrl Pts',(1.80411241501588E-16,-1.12356026268968,
-1.53523027623947E-16));
#13108=CARTESIAN_POINT('Ctrl Pts',(7.41078168374529E-10,-1.14141522098415,
-1.3067981184062E-11));
#13109=CARTESIAN_POINT('Ctrl Pts',(0.00163694718329378,-1.15920272117896,
-1.78823819589733E-6));
#13110=CARTESIAN_POINT('Ctrl Pts',(0.00481087395297265,-1.17671209893291,
-2.3181425555783E-6));
#13111=CARTESIAN_POINT('Ctrl Pts',(0.00802138847203439,-1.19442331774104,
-2.85415543927884E-6));
#13112=CARTESIAN_POINT('Ctrl Pts',(0.0128049030182357,-1.21185152247087,
-2.04128886843626E-6));
#13113=CARTESIAN_POINT('Ctrl Pts',(0.0191087770915565,-1.22877027194193,
1.71240493184593E-7));
#13114=CARTESIAN_POINT('Ctrl Pts',(0.0202201941454154,-1.23175316571065,
5.613248819379E-7));
#13115=CARTESIAN_POINT('Ctrl Pts',(0.0213789882593307,-1.23472016785247,
9.85829603970989E-7));
#13116=CARTESIAN_POINT('Ctrl Pts',(0.0225850188675993,-1.23766995297306,
1.43287414332239E-6));
#13117=CARTESIAN_POINT('Ctrl Pts',(0.0294291562303479,-1.25440977235863,
3.96981990042924E-6));
#13118=CARTESIAN_POINT('Ctrl Pts',(0.0377300686697735,-1.27044838970616,
7.55798501181421E-6));
#13119=CARTESIAN_POINT('Ctrl Pts',(0.0474121614036163,-1.28556782977674,
8.05058320302158E-6));
#13120=CARTESIAN_POINT('Ctrl Pts',(0.0511425121829324,-1.29139310088294,
8.24037316857697E-6));
#13121=CARTESIAN_POINT('Ctrl Pts',(0.0550784035723718,-1.29708174651376,
7.93435480917585E-6));
#13122=CARTESIAN_POINT('Ctrl Pts',(0.0592173503759339,-1.30262033374061,
6.74858081742264E-6));
#13123=CARTESIAN_POINT('Ctrl Pts',(0.0675201807396794,-1.31373087764993,
4.36988865960166E-6));
#13124=CARTESIAN_POINT('Ctrl Pts',(0.0766394565597649,-1.32423847988766,
-1.46587651676554E-6));
#13125=CARTESIAN_POINT('Ctrl Pts',(0.0864911062490747,-1.33409287340636,
-7.46705500292641E-6));
#13126=CARTESIAN_POINT('Ctrl Pts',(0.0992988409846585,-1.34690417528452,
-1.52689465211603E-5));
#13127=CARTESIAN_POINT('Ctrl Pts',(0.113232871116931,-1.35850278376499,
-2.31308069859054E-5));
#13128=CARTESIAN_POINT('Ctrl Pts',(0.128081622025101,-1.36880445085772,
-2.72849174168177E-5));
#13129=CARTESIAN_POINT('Ctrl Pts',(0.142447925282442,-1.37877140864598,
-3.13040575171566E-5));
#13130=CARTESIAN_POINT('Ctrl Pts',(0.157671864768995,-1.38752483454192,
-3.1899138628041E-5));
#13131=CARTESIAN_POINT('Ctrl Pts',(0.173588691395025,-1.39495074934422,
-2.90326641197332E-5));
#13132=CARTESIAN_POINT('Ctrl Pts',(0.189936400238013,-1.40257769006131,
-2.60885916756054E-5));
#13133=CARTESIAN_POINT('Ctrl Pts',(0.206881864105471,-1.40874232120582,
-1.95409011442111E-5));
#13134=CARTESIAN_POINT('Ctrl Pts',(0.22423558959196,-1.41334558507228,-1.29462590315495E-5));
#13135=CARTESIAN_POINT('Ctrl Pts',(0.241260467995769,-1.4178616186841,-6.47658310103417E-6));
#13136=CARTESIAN_POINT('Ctrl Pts',(0.258679581942429,-1.42087546890512,
-1.12101563992788E-10));
#13137=CARTESIAN_POINT('Ctrl Pts',(0.27632692456468,-1.42224670711126,1.05818132034585E-16));
#13138=CARTESIAN_POINT('',(0.,-1.4,0.));
#13139=CARTESIAN_POINT('',(0.292382661757373,-1.22257596919059,0.));
#13140=CARTESIAN_POINT('Ctrl Pts',(0.200274469199584,-1.12301388185427,
-2.68882138776405E-17));
#13141=CARTESIAN_POINT('Ctrl Pts',(0.200274469314753,-1.13095194822878,
-2.85686379674833E-12));
#13142=CARTESIAN_POINT('Ctrl Pts',(0.201244085522878,-1.13884856843413,
-1.08105759021766E-6));
#13143=CARTESIAN_POINT('Ctrl Pts',(0.203110344361254,-1.14653799330522,
-1.10782444979703E-6));
#13144=CARTESIAN_POINT('Ctrl Pts',(0.204308287281872,-1.15147379958167,
-1.12500597321754E-6));
#13145=CARTESIAN_POINT('Ctrl Pts',(0.205876831658669,-1.15632444796435,
-7.573778542164E-7));
#13146=CARTESIAN_POINT('Ctrl Pts',(0.207807574899602,-1.16104329283393,
-1.57887042599725E-7));
#13147=CARTESIAN_POINT('Ctrl Pts',(0.21096922807971,-1.1687705506961,8.23798139982571E-7));
#13148=CARTESIAN_POINT('Ctrl Pts',(0.215060220496011,-1.17605061753432,
2.67511715935828E-6));
#13149=CARTESIAN_POINT('Ctrl Pts',(0.220020901709485,-1.18268777995331,
1.20301732358232E-6));
#13150=CARTESIAN_POINT('Ctrl Pts',(0.222788929945646,-1.18639127392786,
3.81595076007225E-7));
#13151=CARTESIAN_POINT('Ctrl Pts',(0.225828882930032,-1.18989419630164,
-1.55522758636672E-6));
#13152=CARTESIAN_POINT('Ctrl Pts',(0.229112809647272,-1.19317965616817,
-3.52099818518546E-6));
#13153=CARTESIAN_POINT('Ctrl Pts',(0.234731790749985,-1.1988012605745,-6.88454091865859E-6));
#13154=CARTESIAN_POINT('Ctrl Pts',(0.240999377733319,-1.20372479786492,
-1.00686973618824E-5));
#13155=CARTESIAN_POINT('Ctrl Pts',(0.247759525934523,-1.2078808899968,-1.07387199666626E-5));
#13156=CARTESIAN_POINT('Ctrl Pts',(0.251104201987095,-1.20993717358883,
-1.10702228411842E-5));
#13157=CARTESIAN_POINT('Ctrl Pts',(0.254570062984725,-1.21180502729412,
-1.08478245319173E-5));
#13158=CARTESIAN_POINT('Ctrl Pts',(0.258140701417296,-1.21347208138814,
-1.01264154182862E-5));
#13159=CARTESIAN_POINT('Ctrl Pts',(0.265309933881728,-1.21681924144269,
-8.67794906268977E-6));
#13160=CARTESIAN_POINT('Ctrl Pts',(0.27282354441991,-1.21932394229889,-5.03816435877804E-6));
#13161=CARTESIAN_POINT('Ctrl Pts',(0.280540402387729,-1.22090470300999,
-2.38011023443526E-6));
#13162=CARTESIAN_POINT('Ctrl Pts',(0.284441227387562,-1.22170376798259,
-1.03647996128718E-6));
#13163=CARTESIAN_POINT('Ctrl Pts',(0.288394358015454,-1.22226603782358,
-8.41267709508591E-12));
#13164=CARTESIAN_POINT('Ctrl Pts',(0.292382661757373,-1.22257596919059,
3.10081821330854E-17));
#13165=CARTESIAN_POINT('',(0.9,-1.266106713614,0.));
#13166=CARTESIAN_POINT('Ctrl Pts',(0.29238266175737,-1.22257596919059,3.4274341177698E-16));
#13167=CARTESIAN_POINT('Ctrl Pts',(0.494894519961671,-1.23831317320793,
3.6654050078524E-12));
#13168=CARTESIAN_POINT('Ctrl Pts',(0.697432753591781,-1.25280566766171,
-2.10377631034678E-8));
#13169=CARTESIAN_POINT('Ctrl Pts',(0.900000000000002,-1.266106713614,4.80511808774455E-17));
#13170=CARTESIAN_POINT('',(0.9,1.34328341716202,0.));
#13171=CARTESIAN_POINT('',(3.5,-1.37552980833516,0.));
#13172=CARTESIAN_POINT('Ctrl Pts',(1.10000000028363,-1.27885335028943,-5.13283219638443E-11));
#13173=CARTESIAN_POINT('Ctrl Pts',(1.8994825293422,-1.32827224294784,2.51289069808066E-7));
#13174=CARTESIAN_POINT('Ctrl Pts',(2.69943073922525,-1.35940904940056,2.35357980118634E-7));
#13175=CARTESIAN_POINT('Ctrl Pts',(3.50000000097418,-1.37552980835478,8.59034485311056E-16));
#13176=CARTESIAN_POINT('',(3.5,1.44777777777778,0.));
#13177=CARTESIAN_POINT('',(7.1,-1.35793097395724,0.));
#13178=CARTESIAN_POINT('Ctrl Pts',(3.700000000362,-1.379246395385,-6.25385501848083E-12));
#13179=CARTESIAN_POINT('Ctrl Pts',(4.26467016042339,-1.38886773733237,1.63880713394601E-8));
#13180=CARTESIAN_POINT('Ctrl Pts',(4.82965558050887,-1.39115503781354,-4.12727732537403E-8));
#13181=CARTESIAN_POINT('Ctrl Pts',(5.39500817395676,-1.38725486475042,-3.97626883737645E-8));
#13182=CARTESIAN_POINT('Ctrl Pts',(5.96336684492344,-1.38333395379258,-3.82445741104923E-8));
#13183=CARTESIAN_POINT('Ctrl Pts',(6.53173538886785,-1.37316170188981,3.71969681223073E-9));
#13184=CARTESIAN_POINT('Ctrl Pts',(7.1000000000396,-1.35793097389613,-4.88946831112289E-12));
#13185=CARTESIAN_POINT('',(7.1,1.42555555555556,0.));
#13186=CARTESIAN_POINT('',(10.2,-1.23178301601145,0.));
#13187=CARTESIAN_POINT('',(10.5052647440597,-1.21555035534119,0.));
#13188=CARTESIAN_POINT('Ctrl Pts',(10.2,-1.23178301601145,-4.56855690431079E-17));
#13189=CARTESIAN_POINT('Ctrl Pts',(10.3017652114452,-1.22646242153193,-6.28718440835499E-11));
#13190=CARTESIAN_POINT('Ctrl Pts',(10.4035203469111,-1.22104923788321,1.43982679105611E-13));
#13191=CARTESIAN_POINT('Ctrl Pts',(10.5052647440597,-1.21555035534119,6.44897004721534E-17));
#13192=CARTESIAN_POINT('',(10.5997255308004,-1.11583328740478,1.38777878078145E-17));
#13193=CARTESIAN_POINT('Ctrl Pts',(10.5052647440597,-1.21555035534119,-1.86482773667507E-17));
#13194=CARTESIAN_POINT('Ctrl Pts',(10.5131888530666,-1.21512208850275,-5.60416335832109E-13));
#13195=CARTESIAN_POINT('Ctrl Pts',(10.5210180054001,-1.21372544600509,-1.35972994235015E-6));
#13196=CARTESIAN_POINT('Ctrl Pts',(10.5285917824072,-1.2114444991589,-1.66070161277884E-6));
#13197=CARTESIAN_POINT('Ctrl Pts',(10.5334522234388,-1.20998071066451,-1.8538489757029E-6));
#13198=CARTESIAN_POINT('Ctrl Pts',(10.538207639053,-1.20815156029678,-1.66445033219183E-6));
#13199=CARTESIAN_POINT('Ctrl Pts',(10.542812250732,-1.20596855068549,-1.19054254011085E-6));
#13200=CARTESIAN_POINT('Ctrl Pts',(10.5499808226381,-1.20256998801374,-4.52751316616249E-7));
#13201=CARTESIAN_POINT('Ctrl Pts',(10.5567010840309,-1.19835579238971,1.16775294480959E-6));
#13202=CARTESIAN_POINT('Ctrl Pts',(10.5628099082467,-1.1933896765605,3.12218506849373E-7));
#13203=CARTESIAN_POINT('Ctrl Pts',(10.563392699667,-1.1929159013142,2.30599178383296E-7));
#13204=CARTESIAN_POINT('Ctrl Pts',(10.563969906567,-1.19243524850296,1.23643260424227E-7));
#13205=CARTESIAN_POINT('Ctrl Pts',(10.5645413730323,-1.19194775268147,-1.33988689923433E-8));
#13206=CARTESIAN_POINT('Ctrl Pts',(10.5677990734116,-1.18916873515523,-7.94620907596477E-7));
#13207=CARTESIAN_POINT('Ctrl Pts',(10.5708705204042,-1.18616755700159,-2.52696578471864E-6));
#13208=CARTESIAN_POINT('Ctrl Pts',(10.5737438185805,-1.18296717200411,-4.3349897000341E-6));
#13209=CARTESIAN_POINT('Ctrl Pts',(10.579054042416,-1.17705244973962,-7.67644996655303E-6));
#13210=CARTESIAN_POINT('Ctrl Pts',(10.5836289246435,-1.17052745137283,-1.0999028846932E-5));
#13211=CARTESIAN_POINT('Ctrl Pts',(10.5874112735695,-1.16355342251842,-1.18035167459916E-5));
#13212=CARTESIAN_POINT('Ctrl Pts',(10.5894705469099,-1.15975646143,-1.22415145393192E-5));
#13213=CARTESIAN_POINT('Ctrl Pts',(10.5912942421259,-1.15582570378367,-1.20038889321768E-5));
#13214=CARTESIAN_POINT('Ctrl Pts',(10.5928674986933,-1.15178403025788,-1.11465830745351E-5));
#13215=CARTESIAN_POINT('Ctrl Pts',(10.5957384082276,-1.14440870489779,-9.58215448007377E-6));
#13216=CARTESIAN_POINT('Ctrl Pts',(10.5977463817932,-1.13674651935037,-5.80208140981121E-6));
#13217=CARTESIAN_POINT('Ctrl Pts',(10.5988207707371,-1.12894377506163,-2.8960211281105E-6));
#13218=CARTESIAN_POINT('Ctrl Pts',(10.5994175893465,-1.12460938291963,-1.28171667533415E-6));
#13219=CARTESIAN_POINT('Ctrl Pts',(10.5997255306822,-1.12023121224821,-9.4020583932734E-12));
#13220=CARTESIAN_POINT('Ctrl Pts',(10.5997255308004,-1.11583328740478,-9.97465998686664E-18));
#13221=CARTESIAN_POINT('',(10.5997255308004,1.11583328740478,0.));
#13222=CARTESIAN_POINT('',(10.5997255308004,0.7,0.));
#13223=CARTESIAN_POINT('',(10.5052647440597,1.21555035534119,0.));
#13224=CARTESIAN_POINT('Ctrl Pts',(10.5997255308004,1.11583328740478,8.8037216405823E-17));
#13225=CARTESIAN_POINT('Ctrl Pts',(10.5997255307124,1.12376989384288,-2.22024716398596E-12));
#13226=CARTESIAN_POINT('Ctrl Pts',(10.5987536115518,1.13166401228391,-1.27532141444775E-6));
#13227=CARTESIAN_POINT('Ctrl Pts',(10.5968849989732,1.13935090273995,-1.5236651967046E-6));
#13228=CARTESIAN_POINT('Ctrl Pts',(10.5956849616024,1.14428748291596,-1.68315348385219E-6));
#13229=CARTESIAN_POINT('Ctrl Pts',(10.5941139374364,1.14913880701507,-1.46899737395989E-6));
#13230=CARTESIAN_POINT('Ctrl Pts',(10.5921809408638,1.1538584293407,-9.90118991603547E-7));
#13231=CARTESIAN_POINT('Ctrl Pts',(10.5891742477341,1.16119959911942,-2.45244239835432E-7));
#13232=CARTESIAN_POINT('Ctrl Pts',(10.5853292249979,1.16813727090899,1.33309554558619E-6));
#13233=CARTESIAN_POINT('Ctrl Pts',(10.5807005079991,1.17450509276749,4.08358240744415E-7));
#13234=CARTESIAN_POINT('Ctrl Pts',(10.5802604812716,1.17511044665166,3.20448539159982E-7));
#13235=CARTESIAN_POINT('Ctrl Pts',(10.5798133373602,1.17571063303672,2.07176952714776E-7));
#13236=CARTESIAN_POINT('Ctrl Pts',(10.5793591019426,1.17630549598644,6.38823567561716E-8));
#13237=CARTESIAN_POINT('Ctrl Pts',(10.5767566952267,1.17971358631841,-7.57081408668461E-7));
#13238=CARTESIAN_POINT('Ctrl Pts',(10.5739217504488,1.18294722379721,-2.53660858190298E-6));
#13239=CARTESIAN_POINT('Ctrl Pts',(10.570876618072,1.18599321478588,-4.38998728286835E-6));
#13240=CARTESIAN_POINT('Ctrl Pts',(10.5652565693637,1.19161484813492,-7.81055403847458E-6));
#13241=CARTESIAN_POINT('Ctrl Pts',(10.5589874561388,1.19653507038546,-1.11999964534866E-5));
#13242=CARTESIAN_POINT('Ctrl Pts',(10.5522271124844,1.20068789486255,-1.20263298844839E-5));
#13243=CARTESIAN_POINT('Ctrl Pts',(10.5485500617744,1.20294667739977,-1.24757848359648E-5));
#13244=CARTESIAN_POINT('Ctrl Pts',(10.5447269560479,1.20497781184918,-1.22374322375965E-5));
#13245=CARTESIAN_POINT('Ctrl Pts',(10.5407797717187,1.20676523914267,-1.13674773191707E-5));
#13246=CARTESIAN_POINT('Ctrl Pts',(10.5335711832013,1.210029547771,-9.77871264224002E-6));
#13247=CARTESIAN_POINT('Ctrl Pts',(10.5260296312848,1.21244761587922,-5.9245235663186E-6));
#13248=CARTESIAN_POINT('Ctrl Pts',(10.5182973307397,1.21394093281975,-2.95733858081469E-6));
#13249=CARTESIAN_POINT('Ctrl Pts',(10.514004731837,1.21476995008607,-1.31010113336685E-6));
#13250=CARTESIAN_POINT('Ctrl Pts',(10.5096528988527,1.21531319279956,-7.28166367327128E-12));
#13251=CARTESIAN_POINT('Ctrl Pts',(10.5052647440597,1.21555035534119,-3.31765864780564E-17));
#13252=CARTESIAN_POINT('',(10.2,1.23178301601145,0.));
#13253=CARTESIAN_POINT('Ctrl Pts',(10.5052647440597,1.21555035534119,1.20285454773689E-16));
#13254=CARTESIAN_POINT('Ctrl Pts',(10.4035203468995,1.22104923788384,1.44021921739714E-13));
#13255=CARTESIAN_POINT('Ctrl Pts',(10.3017652114309,1.22646242153268,-6.28696045710378E-11));
#13256=CARTESIAN_POINT('Ctrl Pts',(10.2,1.23178301601145,1.23125603768043E-16));
#13257=CARTESIAN_POINT('',(10.2,-1.30754691548544,0.));
#13258=CARTESIAN_POINT('Origin',(8.8,0.,0.));
#13259=CARTESIAN_POINT('',(8.4,-4.89858719658942E-17,0.));
#13260=CARTESIAN_POINT('Origin',(2.,0.,0.));
#13261=CARTESIAN_POINT('',(1.6,-4.89858719658941E-17,0.7));
#13262=CARTESIAN_POINT('Origin',(2.,0.,0.7));
#13263=CARTESIAN_POINT('',(1.6,-4.89858719658941E-17,0.));
#13264=CARTESIAN_POINT('Origin',(10.2,-1.30754691548544,0.));
#13265=CARTESIAN_POINT('',(10.1999999975107,-1.19856231453552,0.605472757505173));
#13266=CARTESIAN_POINT('Ctrl Pts',(10.2,-1.23178301601145,0.));
#13267=CARTESIAN_POINT('Ctrl Pts',(10.2,-1.22625045235593,0.100869147801815));
#13268=CARTESIAN_POINT('Ctrl Pts',(10.2,-1.22071692450357,0.201739022585575));
#13269=CARTESIAN_POINT('Ctrl Pts',(10.2,-1.2096433936729,0.403562754186249));
#13270=CARTESIAN_POINT('Ctrl Pts',(10.1999999975107,-1.20410330368611,0.50451817268257));
#13271=CARTESIAN_POINT('Ctrl Pts',(10.1999999975107,-1.19856231453552,0.605472757505173));
#13272=CARTESIAN_POINT('',(10.1999999975107,1.19856231453552,0.605472757505173));
#13273=CARTESIAN_POINT('Ctrl Pts',(10.1999999975107,1.19856231453552,0.605472757505173));
#13274=CARTESIAN_POINT('Ctrl Pts',(10.1999999975107,1.20410418062036,0.504502195294633));
#13275=CARTESIAN_POINT('Ctrl Pts',(10.2,1.20964514726505,0.403530798997214));
#13276=CARTESIAN_POINT('Ctrl Pts',(10.2,1.22071867750565,0.201707067365009));
#13277=CARTESIAN_POINT('Ctrl Pts',(10.2,1.22625132869937,0.100853170395858));
#13278=CARTESIAN_POINT('Ctrl Pts',(10.2,1.23178301601145,0.));
#13279=CARTESIAN_POINT('',(10.1999999980542,1.09857320530976,0.7));
#13280=CARTESIAN_POINT('Ctrl Pts',(10.1999999999973,1.09857320510493,0.7));
#13281=CARTESIAN_POINT('Ctrl Pts',(10.2000000008642,1.10649088744708,0.699999999248278));
#13282=CARTESIAN_POINT('Ctrl Pts',(10.1999989363772,1.11434529358656,0.699006164779054));
#13283=CARTESIAN_POINT('Ctrl Pts',(10.1999980093114,1.12199598895487,0.697118997523365));
#13284=CARTESIAN_POINT('Ctrl Pts',(10.1999974900707,1.12628106973794,0.696062013320951));
#13285=CARTESIAN_POINT('Ctrl Pts',(10.1999970168623,1.13050229860485,0.694723760583242));
#13286=CARTESIAN_POINT('Ctrl Pts',(10.199996713894,1.13463332887353,0.693115046692397));
#13287=CARTESIAN_POINT('Ctrl Pts',(10.1999961690675,1.14206214329588,0.690222103243312));
#13288=CARTESIAN_POINT('Ctrl Pts',(10.1999962772589,1.14911941279843,0.686488866209959));
#13289=CARTESIAN_POINT('Ctrl Pts',(10.1999969599022,1.15565885618684,0.681996408643444));
#13290=CARTESIAN_POINT('Ctrl Pts',(10.1999973343062,1.15924549304116,0.679532465931891));
#13291=CARTESIAN_POINT('Ctrl Pts',(10.1999978674396,1.16267609380848,0.676839263748528));
#13292=CARTESIAN_POINT('Ctrl Pts',(10.1999983417863,1.16592263776853,0.673924718551186));
#13293=CARTESIAN_POINT('Ctrl Pts',(10.199998806773,1.16910511991263,0.671067684066867));
#13294=CARTESIAN_POINT('Ctrl Pts',(10.1999992207276,1.17209141256199,0.668015240668471));
#13295=CARTESIAN_POINT('Ctrl Pts',(10.1999992206607,1.17485880184773,0.664778864469812));
#13296=CARTESIAN_POINT('Ctrl Pts',(10.1999992205369,1.17997899231675,0.658790960038769));
#13297=CARTESIAN_POINT('Ctrl Pts',(10.1999979581638,1.18435276586188,0.652174799271591));
#13298=CARTESIAN_POINT('Ctrl Pts',(10.1999975326045,1.18791964688485,0.645095405674036));
#13299=CARTESIAN_POINT('Ctrl Pts',(10.1999974898604,1.18827791229431,0.644384335742179));
#13300=CARTESIAN_POINT('Ctrl Pts',(10.1999974535047,1.18862799840101,0.643668573506599));
#13301=CARTESIAN_POINT('Ctrl Pts',(10.1999974242393,1.18896981696374,0.64294827577739));
#13302=CARTESIAN_POINT('Ctrl Pts',(10.1999971329942,1.1923715530028,0.635779961907205));
#13303=CARTESIAN_POINT('Ctrl Pts',(10.1999977790614,1.19491900203126,0.628247233077589));
#13304=CARTESIAN_POINT('Ctrl Pts',(10.1999987199397,1.19655829940385,0.620518158911201));
#13305=CARTESIAN_POINT('Ctrl Pts',(10.1999993222661,1.19760773597399,0.615570201805241));
#13306=CARTESIAN_POINT('Ctrl Pts',(10.2,1.19828413277105,0.610541112135461));
#13307=CARTESIAN_POINT('Ctrl Pts',(10.2,1.19856231427281,0.60547275750556));
#13308=CARTESIAN_POINT('',(10.2,-1.09857320510402,0.7));
#13309=CARTESIAN_POINT('',(10.2,-0.653773457742722,0.7));
#13310=CARTESIAN_POINT('Ctrl Pts',(10.2,-1.19856231427281,0.60547275750556));
#13311=CARTESIAN_POINT('Ctrl Pts',(10.2,-1.19812809376428,0.613384079828744));
#13312=CARTESIAN_POINT('Ctrl Pts',(10.1999984889428,-1.1967261327477,0.621202329970501));
#13313=CARTESIAN_POINT('Ctrl Pts',(10.1999978161146,-1.19444079525024,0.628767398200536));
#13314=CARTESIAN_POINT('Ctrl Pts',(10.1999974438306,-1.19317629038787,0.632953241898348));
#13315=CARTESIAN_POINT('Ctrl Pts',(10.1999972759003,-1.19164034846853,0.637061602680377));
#13316=CARTESIAN_POINT('Ctrl Pts',(10.1999973648938,-1.18984073583679,0.641063423920242));
#13317=CARTESIAN_POINT('Ctrl Pts',(10.1999975257516,-1.18658789218766,0.648296813248274));
#13318=CARTESIAN_POINT('Ctrl Pts',(10.1999986492083,-1.18251199594868,0.655103972585077));
#13319=CARTESIAN_POINT('Ctrl Pts',(10.1999990866637,-1.1776776067306,0.66132208754656));
#13320=CARTESIAN_POINT('Ctrl Pts',(10.1999991692372,-1.17676507450965,0.662495809810115));
#13321=CARTESIAN_POINT('Ctrl Pts',(10.1999992204458,-1.17582538639523,0.663648473741297));
#13322=CARTESIAN_POINT('Ctrl Pts',(10.1999992199672,-1.17485880188435,0.664778864469789));
#13323=CARTESIAN_POINT('Ctrl Pts',(10.1999992190419,-1.17299032792757,0.666963987046661));
#13324=CARTESIAN_POINT('Ctrl Pts',(10.1999990265713,-1.17102137903347,0.669065925022507));
#13325=CARTESIAN_POINT('Ctrl Pts',(10.1999987631451,-1.16895889720817,0.671081139337088));
#13326=CARTESIAN_POINT('Ctrl Pts',(10.1999980371048,-1.16327440276409,0.676635357771578));
#13327=CARTESIAN_POINT('Ctrl Pts',(10.1999968952367,-1.15694629605269,0.681471105251756));
#13328=CARTESIAN_POINT('Ctrl Pts',(10.1999965193249,-1.15013861030111,0.685534582868085));
#13329=CARTESIAN_POINT('Ctrl Pts',(10.1999962798276,-1.14580136285465,0.688123466749966));
#13330=CARTESIAN_POINT('Ctrl Pts',(10.1999963003895,-1.14126848503633,0.690398200126003));
#13331=CARTESIAN_POINT('Ctrl Pts',(10.1999965837416,-1.13657664085124,0.692335536714198));
#13332=CARTESIAN_POINT('Ctrl Pts',(10.199997026059,-1.12925259320479,0.695359751696499));
#13333=CARTESIAN_POINT('Ctrl Pts',(10.1999981114625,-1.12162598460505,0.697529439192009));
#13334=CARTESIAN_POINT('Ctrl Pts',(10.1999989867727,-1.11384404680861,0.698775198878229));
#13335=CARTESIAN_POINT('Ctrl Pts',(10.1999995533653,-1.10880676031141,0.699581585232154));
#13336=CARTESIAN_POINT('Ctrl Pts',(10.200000000559,-1.10370379302489,0.699999999512891));
#13337=CARTESIAN_POINT('Ctrl Pts',(10.1999999999973,-1.09857320510493,0.7));
#13338=CARTESIAN_POINT('Ctrl Pts',(10.0273290644374,-1.24073895154929,-0.000342977371441382));
#13339=CARTESIAN_POINT('Ctrl Pts',(10.0182194939277,-1.2301570933055,0.201590462913323));
#13340=CARTESIAN_POINT('Ctrl Pts',(10.0091098064739,-1.21957524432673,0.403523898419685));
#13341=CARTESIAN_POINT('Ctrl Pts',(10.,-1.20899340483173,0.605457329065658));
#13342=CARTESIAN_POINT('Ctrl Pts',(9.11786336174441,-1.287320026752,-0.000205293215301774));
#13343=CARTESIAN_POINT('Ctrl Pts',(9.11054075262461,-1.27673792859995,0.201728409731728));
#13344=CARTESIAN_POINT('Ctrl Pts',(9.10321803982027,-1.2661558351744,0.403662109352091));
#13345=CARTESIAN_POINT('Ctrl Pts',(9.09589522044064,-1.25557375159922,0.605595805683776));
#13346=CARTESIAN_POINT('Ctrl Pts',(8.20875307681921,-1.32613868191631,-8.19769783003664E-5));
#13347=CARTESIAN_POINT('Ctrl Pts',(8.20321812688803,-1.31555630757271,0.201851960079368));
#13348=CARTESIAN_POINT('Ctrl Pts',(8.19768309032111,-1.30497393555236,0.403785895133155));
#13349=CARTESIAN_POINT('Ctrl Pts',(8.19214796413157,-1.29439157095064,0.605719828258773));
#13350=CARTESIAN_POINT('Ctrl Pts',(7.29999999999999,-1.35236351479115,1.04083408558608E-17));
#13351=CARTESIAN_POINT('Ctrl Pts',(7.29625341766944,-1.34178092325774,0.201934092022114));
#13352=CARTESIAN_POINT('Ctrl Pts',(7.2925067690755,-1.33119833465137,0.403868182971915));
#13353=CARTESIAN_POINT('Ctrl Pts',(7.28876005303739,-1.32061574904145,0.605802272831199));
#13354=CARTESIAN_POINT('Ctrl Pts',(7.29999999953094,-1.32031613471704,0.605285370449856));
#13355=CARTESIAN_POINT('Ctrl Pts',(8.20058408060299,-1.29406305600824,0.605326635812744));
#13356=CARTESIAN_POINT('Ctrl Pts',(9.10058974048747,-1.25534320916473,0.605388449123016));
#13357=CARTESIAN_POINT('Ctrl Pts',(9.99999999968202,-1.20899340489109,0.605457329065633));
#13358=CARTESIAN_POINT('Ctrl Pts',(10.5052670937641,-1.21555282972197,-4.72190879230918E-5));
#13359=CARTESIAN_POINT('Ctrl Pts',(10.4952228315222,-1.20497561405085,0.201799837144789));
#13360=CARTESIAN_POINT('Ctrl Pts',(10.4851784461209,-1.19439840869387,0.403646887802288));
#13361=CARTESIAN_POINT('Ctrl Pts',(10.4751339353761,-1.18382121389426,0.605493932788863));
#13362=CARTESIAN_POINT('Ctrl Pts',(10.4035069533234,-1.22105168617584,-3.13467776074076E-5));
#13363=CARTESIAN_POINT('Ctrl Pts',(10.3936624949941,-1.21047444506522,0.201815739766394));
#13364=CARTESIAN_POINT('Ctrl Pts',(10.3838179147697,-1.19989721405033,0.403662820908308));
#13365=CARTESIAN_POINT('Ctrl Pts',(10.3739732104882,-1.18931999337004,0.605509896555428));
#13366=CARTESIAN_POINT('Ctrl Pts',(10.3017512542637,-1.22646400658821,-1.55943981238903E-5));
#13367=CARTESIAN_POINT('Ctrl Pts',(10.2921066085356,-1.21588673949083,0.201831522212972));
#13368=CARTESIAN_POINT('Ctrl Pts',(10.2824618422276,-1.20530948226626,0.403678633593635));
#13369=CARTESIAN_POINT('Ctrl Pts',(10.2728169532007,-1.19473223514815,0.605525739654126));
#13370=CARTESIAN_POINT('Ctrl Pts',(10.2,-1.23178301601145,-4.5102810375397E-17));
#13371=CARTESIAN_POINT('Ctrl Pts',(10.1905551755811,-1.22120572247414,0.20184714636246));
#13372=CARTESIAN_POINT('Ctrl Pts',(10.1811102319487,-1.21062843858304,0.403694287664275));
#13373=CARTESIAN_POINT('Ctrl Pts',(10.1716651669877,-1.20005116456574,0.605541423818621));
#13374=CARTESIAN_POINT('',(10.4735630903435,-1.18390659316268,0.605494180667944));
#13375=CARTESIAN_POINT('Ctrl Pts',(10.1999999975038,-1.19856231440453,0.605472757505366));
#13376=CARTESIAN_POINT('Ctrl Pts',(10.2911933328565,-1.19375025772558,0.605479840815741));
#13377=CARTESIAN_POINT('Ctrl Pts',(10.3823809652617,-1.18886335120032,0.605486986548286));
#13378=CARTESIAN_POINT('Ctrl Pts',(10.4735630903435,-1.18390659316268,0.605494180667944));
#13379=CARTESIAN_POINT('Ctrl Pts',(10.4735630903435,-1.18390659316268,0.605494180667945));
#13380=CARTESIAN_POINT('Ctrl Pts',(10.4841302498201,-1.19445434834508,0.403662775875149));
#13381=CARTESIAN_POINT('Ctrl Pts',(10.4946974680575,-1.20500226999407,0.201831382381129));
#13382=CARTESIAN_POINT('Ctrl Pts',(10.5052647440597,-1.21555035534119,-6.86299975183324E-17));
#13383=CARTESIAN_POINT('Ctrl Pts',(10.,-1.10900986674273,0.7));
#13384=CARTESIAN_POINT('Ctrl Pts',(9.09944331332257,-1.15544418981837,0.7));
#13385=CARTESIAN_POINT('Ctrl Pts',(8.1984670949788,-1.19422430779862,0.7));
#13386=CARTESIAN_POINT('Ctrl Pts',(7.29709043526679,-1.22049830417059,0.7));
#13387=CARTESIAN_POINT('Ctrl Pts',(10.0014871213396,-1.13785139984992,0.7));
#13388=CARTESIAN_POINT('Ctrl Pts',(9.10076698492608,-1.18430758604571,0.700000491839571));
#13389=CARTESIAN_POINT('Ctrl Pts',(8.19957769811723,-1.22310890030201,0.699999704549177));
#13390=CARTESIAN_POINT('Ctrl Pts',(7.29793284700475,-1.24939875264889,0.7));
#13391=CARTESIAN_POINT('Ctrl Pts',(10.0040646682326,-1.18784086746588,0.676686753673613));
#13392=CARTESIAN_POINT('Ctrl Pts',(9.10306300621911,-1.23433322993607,0.676664155483858));
#13393=CARTESIAN_POINT('Ctrl Pts',(8.20149954052229,-1.27317186922949,0.676644146017133));
#13394=CARTESIAN_POINT('Ctrl Pts',(7.29939288958795,-1.29948813715084,0.676630595533454));
#13395=CARTESIAN_POINT('Ctrl Pts',(10.0050807923581,-1.20754778500352,0.627085325222079));
#13396=CARTESIAN_POINT('Ctrl Pts',(9.10396596140607,-1.25402923300358,0.627026849623412));
#13397=CARTESIAN_POINT('Ctrl Pts',(8.20225661204673,-1.29285896783792,0.626974637782525));
#13398=CARTESIAN_POINT('Ctrl Pts',(7.29996660609514,-1.31917051289423,0.626939603849942));
#13399=CARTESIAN_POINT('Ctrl Pts',(10.0051416645797,-1.20872835322339,0.605457722909465));
#13400=CARTESIAN_POINT('Ctrl Pts',(9.1040197884667,-1.25519559703033,0.605388684776982));
#13401=CARTESIAN_POINT('Ctrl Pts',(8.20230020786566,-1.29401302889245,0.605326714446839));
#13402=CARTESIAN_POINT('Ctrl Pts',(7.29999999953094,-1.32031613471704,0.605285370449856));
#13403=CARTESIAN_POINT('Ctrl Pts',(10.4681436286308,-1.08420482079362,0.7));
#13404=CARTESIAN_POINT('Ctrl Pts',(10.3770124662346,-1.0891584122264,0.7));
#13405=CARTESIAN_POINT('Ctrl Pts',(10.285877616441,-1.09404209584202,0.7));
#13406=CARTESIAN_POINT('Ctrl Pts',(10.1947388861048,-1.09885088260188,0.7));
#13407=CARTESIAN_POINT('Ctrl Pts',(10.4697107510168,-1.11303515260326,0.7));
#13408=CARTESIAN_POINT('Ctrl Pts',(10.3785648662465,-1.11799094453753,0.700000051218742));
#13409=CARTESIAN_POINT('Ctrl Pts',(10.2874149314686,-1.12287675076168,0.699999949550842));
#13410=CARTESIAN_POINT('Ctrl Pts',(10.196260416419,-1.12768774893097,0.7));
#13411=CARTESIAN_POINT('Ctrl Pts',(10.4724269697127,-1.16300539549315,0.676698381019543));
#13412=CARTESIAN_POINT('Ctrl Pts',(10.3812557252598,-1.16796482352885,0.676696026813929));
#13413=CARTESIAN_POINT('Ctrl Pts',(10.2900793016129,-1.17285439035486,0.676693724638983));
#13414=CARTESIAN_POINT('Ctrl Pts',(10.1988975981852,-1.17766904563614,0.67669140632491));
#13415=CARTESIAN_POINT('Ctrl Pts',(10.4734985149421,-1.18271860027509,0.627116141711795));
#13416=CARTESIAN_POINT('Ctrl Pts',(10.382317043787,-1.18767684023183,0.627110048826767));
#13417=CARTESIAN_POINT('Ctrl Pts',(10.2911301919381,-1.19256517083271,0.627104033151799));
#13418=CARTESIAN_POINT('Ctrl Pts',(10.1999375452555,-1.19737868557977,0.627098033786781));
#13419=CARTESIAN_POINT('Ctrl Pts',(10.4735630903435,-1.18390659316268,0.605494180667944));
#13420=CARTESIAN_POINT('Ctrl Pts',(10.3823809652617,-1.18886335120032,0.605486986548286));
#13421=CARTESIAN_POINT('Ctrl Pts',(10.2911933328565,-1.19375025772558,0.605479840815741));
#13422=CARTESIAN_POINT('Ctrl Pts',(10.1999999975038,-1.19856231440453,0.605472757505366));
#13423=CARTESIAN_POINT('',(10.4681436258201,-1.08420482094639,0.7));
#13424=CARTESIAN_POINT('Ctrl Pts',(10.4681436258201,-1.0842048209464,0.7));
#13425=CARTESIAN_POINT('Ctrl Pts',(10.3787660248044,-1.08906309452597,0.7));
#13426=CARTESIAN_POINT('Ctrl Pts',(10.289384876933,-1.09385412476048,0.7));
#13427=CARTESIAN_POINT('Ctrl Pts',(10.1999999999973,-1.09857320510493,0.7));
#13428=CARTESIAN_POINT('Origin',(10.4681436286308,-1.08420482099672,0.6));
#13429=CARTESIAN_POINT('Origin',(5.4,-8.11656130105013E-18,0.7));
#13430=CARTESIAN_POINT('',(10.4681436286308,1.08420482109828,0.7));
#13431=CARTESIAN_POINT('Ctrl Pts',(10.1999999980461,1.09857320520795,0.7));
#13432=CARTESIAN_POINT('Ctrl Pts',(10.2893848765692,1.09385412478074,0.7));
#13433=CARTESIAN_POINT('Ctrl Pts',(10.3787660260279,1.08906309446088,0.7));
#13434=CARTESIAN_POINT('Ctrl Pts',(10.4681436286308,1.08420482079361,0.7));
#13435=CARTESIAN_POINT('',(10.4681436286308,0.7,0.7));
#13436=CARTESIAN_POINT('Ctrl Pts',(7.3,1.35236351479305,-3.57463069561303E-11));
#13437=CARTESIAN_POINT('Ctrl Pts',(7.29625341766908,1.34178092325856,0.20193409200674));
#13438=CARTESIAN_POINT('Ctrl Pts',(7.29250676907475,1.33119833465113,0.403868182976914));
#13439=CARTESIAN_POINT('Ctrl Pts',(7.28876005303626,1.32061574904014,0.60580227285657));
#13440=CARTESIAN_POINT('Ctrl Pts',(8.20875307682014,1.32613868191819,-8.19770140467192E-5));
#13441=CARTESIAN_POINT('Ctrl Pts',(8.20321812688841,1.31555630757352,0.201851960063995));
#13442=CARTESIAN_POINT('Ctrl Pts',(8.19768309032092,1.3049739355521,0.403785895138154));
#13443=CARTESIAN_POINT('Ctrl Pts',(8.19214796413082,1.29439157094932,0.605719828284144));
#13444=CARTESIAN_POINT('Ctrl Pts',(9.11786336174626,1.28732002675385,-0.000205293251048056));
#13445=CARTESIAN_POINT('Ctrl Pts',(9.11054075262572,1.27673792860073,0.201728409716354));
#13446=CARTESIAN_POINT('Ctrl Pts',(9.10321803982063,1.26615583517412,0.403662109357089));
#13447=CARTESIAN_POINT('Ctrl Pts',(9.09589522044026,1.25557375159787,0.605595805709147));
#13448=CARTESIAN_POINT('Ctrl Pts',(10.0273290644402,1.2407389515511,-0.000342977407187712));
#13449=CARTESIAN_POINT('Ctrl Pts',(10.0182194939295,1.23015709330624,0.201590462897949));
#13450=CARTESIAN_POINT('Ctrl Pts',(10.0091098064748,1.21957524432641,0.403523898424684));
#13451=CARTESIAN_POINT('Ctrl Pts',(10.,1.20899340483035,0.605457329091028));
#13452=CARTESIAN_POINT('Ctrl Pts',(10.2,1.23178301601276,-2.39624899783797E-11));
#13453=CARTESIAN_POINT('Ctrl Pts',(10.1905551755807,1.22120572247504,0.201847146346486));
#13454=CARTESIAN_POINT('Ctrl Pts',(10.1811102319479,1.21062843858352,0.403694287656288));
#13455=CARTESIAN_POINT('Ctrl Pts',(10.1716651669865,1.2000511645658,0.605541423818621));
#13456=CARTESIAN_POINT('Ctrl Pts',(10.3017512542641,1.22646400658951,-1.55944220863836E-5));
#13457=CARTESIAN_POINT('Ctrl Pts',(10.2921066085356,1.2158867394917,0.201831522196997));
#13458=CARTESIAN_POINT('Ctrl Pts',(10.2824618422272,1.20530948226672,0.403678633585648));
#13459=CARTESIAN_POINT('Ctrl Pts',(10.2728169531999,1.19473223514819,0.605525739654127));
#13460=CARTESIAN_POINT('Ctrl Pts',(10.4035069533242,1.22105168617711,-3.13468015701665E-5));
#13461=CARTESIAN_POINT('Ctrl Pts',(10.3936624949945,1.21047444506608,0.201815739750419));
#13462=CARTESIAN_POINT('Ctrl Pts',(10.3838179147698,1.19989721405077,0.40366282090032));
#13463=CARTESIAN_POINT('Ctrl Pts',(10.3739732104878,1.18931999337006,0.605509896555428));
#13464=CARTESIAN_POINT('Ctrl Pts',(10.5052670937653,1.21555282972323,-4.72191118859062E-5));
#13465=CARTESIAN_POINT('Ctrl Pts',(10.495222831523,1.20497561405169,0.201799837128814));
#13466=CARTESIAN_POINT('Ctrl Pts',(10.4851784461213,1.19439840869429,0.403646887794301));
#13467=CARTESIAN_POINT('Ctrl Pts',(10.4751339353761,1.18382121389426,0.605493932788864));
#13468=CARTESIAN_POINT('',(10.4735630903435,1.18390659316268,0.605494180667944));
#13469=CARTESIAN_POINT('Ctrl Pts',(10.5052647440597,1.21555035534119,-4.0462425077159E-16));
#13470=CARTESIAN_POINT('Ctrl Pts',(10.4946974680575,1.20500226999407,0.201831382381129));
#13471=CARTESIAN_POINT('Ctrl Pts',(10.4841302498201,1.19445434834508,0.40366277587515));
#13472=CARTESIAN_POINT('Ctrl Pts',(10.4735630903435,1.18390659316268,0.605494180667945));
#13473=CARTESIAN_POINT('Ctrl Pts',(10.4735630903435,1.18390659316268,0.605494180667944));
#13474=CARTESIAN_POINT('Ctrl Pts',(10.3823809652617,1.18886335120032,0.605486986548286));
#13475=CARTESIAN_POINT('Ctrl Pts',(10.2911933328565,1.19375025772558,0.605479840815741));
#13476=CARTESIAN_POINT('Ctrl Pts',(10.1999999975038,1.19856231440453,0.605472757505366));
#13477=CARTESIAN_POINT('Origin',(7.1,1.42555555555556,0.));
#13478=CARTESIAN_POINT('',(7.0999999994629,-1.32593912634735,0.605276549957215));
#13479=CARTESIAN_POINT('Ctrl Pts',(7.0999999994629,-1.32593912634735,0.605276549957215));
#13480=CARTESIAN_POINT('Ctrl Pts',(7.0999999994629,-1.33126650931098,0.504490734647167));
#13481=CARTESIAN_POINT('Ctrl Pts',(7.1,-1.33659376385849,0.403703958452373));
#13482=CARTESIAN_POINT('Ctrl Pts',(7.1,-1.3472576786761,0.201945747207886));
#13483=CARTESIAN_POINT('Ctrl Pts',(7.1,-1.35259443928223,0.100972400854069));
#13484=CARTESIAN_POINT('Ctrl Pts',(7.1,-1.35793097395724,0.));
#13485=CARTESIAN_POINT('',(7.1,-1.22604182196417,0.7));
#13486=CARTESIAN_POINT('Ctrl Pts',(7.1,-1.22604182196307,0.7));
#13487=CARTESIAN_POINT('Ctrl Pts',(7.1,-1.23395163718705,0.7));
#13488=CARTESIAN_POINT('Ctrl Pts',(7.09999945440688,-1.24179783218049,0.699006056038995));
#13489=CARTESIAN_POINT('Ctrl Pts',(7.09999897931553,-1.2494401870438,0.697119011207626));
#13490=CARTESIAN_POINT('Ctrl Pts',(7.09999871186578,-1.25374240366384,0.696056710937424));
#13491=CARTESIAN_POINT('Ctrl Pts',(7.09999846845149,-1.25798007942473,0.69471034534287));
#13492=CARTESIAN_POINT('Ctrl Pts',(7.09999831430822,-1.26212651101681,0.6930909329195));
#13493=CARTESIAN_POINT('Ctrl Pts',(7.09999803835695,-1.26954956016987,0.690191818885951));
#13494=CARTESIAN_POINT('Ctrl Pts',(7.09999810102228,-1.27659977900265,0.686452252582521));
#13495=CARTESIAN_POINT('Ctrl Pts',(7.09999845706054,-1.28313109767173,0.681953977461377));
#13496=CARTESIAN_POINT('Ctrl Pts',(7.09999865314126,-1.2867280867584,0.679476645189077));
#13497=CARTESIAN_POINT('Ctrl Pts',(7.09999893113315,-1.29016742765117,0.67676830886676));
#13498=CARTESIAN_POINT('Ctrl Pts',(7.09999917787259,-1.2934208019838,0.673837071833988));
#13499=CARTESIAN_POINT('Ctrl Pts',(7.09999941835505,-1.29659167515528,0.670980166997299));
#13500=CARTESIAN_POINT('Ctrl Pts',(7.09999963169439,-1.29956664557352,0.667928795646746));
#13501=CARTESIAN_POINT('Ctrl Pts',(7.09999963110542,-1.30232317314677,0.664694459428825));
#13502=CARTESIAN_POINT('Ctrl Pts',(7.09999963001387,-1.30743194453681,0.658700148145236));
#13503=CARTESIAN_POINT('Ctrl Pts',(7.09999897381858,-1.31179333085743,0.652078782729069));
#13504=CARTESIAN_POINT('Ctrl Pts',(7.09999874753952,-1.31534789998199,0.64499600756552));
#13505=CARTESIAN_POINT('Ctrl Pts',(7.09999872438549,-1.31571162172319,0.644271261689237));
#13506=CARTESIAN_POINT('Ctrl Pts',(7.0999987046402,-1.31606685549941,0.643541664816448));
#13507=CARTESIAN_POINT('Ctrl Pts',(7.09999868869212,-1.31641350913238,0.642807383257706));
#13508=CARTESIAN_POINT('Ctrl Pts',(7.09999853283271,-1.31980133087414,0.635631300872562));
#13509=CARTESIAN_POINT('Ctrl Pts',(7.09999885939544,-1.32233451509485,0.628092322434426));
#13510=CARTESIAN_POINT('Ctrl Pts',(7.09999934101855,-1.32395982399511,0.620358959365968));
#13511=CARTESIAN_POINT('Ctrl Pts',(7.09999964997549,-1.32500244522074,0.615398075635307));
#13512=CARTESIAN_POINT('Ctrl Pts',(7.09999999934316,-1.32567060646853,0.610356529630438));
#13513=CARTESIAN_POINT('Ctrl Pts',(7.09999999981141,-1.32593912630714,0.60527654995744));
#13514=CARTESIAN_POINT('',(7.09999999995537,1.22604182196549,0.7));
#13515=CARTESIAN_POINT('',(7.1,0.712777777777778,0.7));
#13516=CARTESIAN_POINT('',(7.0999999994629,1.32593912634735,0.605276549957215));
#13517=CARTESIAN_POINT('Ctrl Pts',(7.09999999981142,1.32593912630714,0.60527654995744));
#13518=CARTESIAN_POINT('Ctrl Pts',(7.09999999908198,1.32552083177145,0.613190035045322));
#13519=CARTESIAN_POINT('Ctrl Pts',(7.09999922367565,1.32413525001942,0.621012727860624));
#13520=CARTESIAN_POINT('Ctrl Pts',(7.09999888117586,1.32186630199077,0.628584136488803));
#13521=CARTESIAN_POINT('Ctrl Pts',(7.09999868987568,1.32059900146923,0.632813078704371));
#13522=CARTESIAN_POINT('Ctrl Pts',(7.09999860640034,1.3190551184949,0.636963663611311));
#13523=CARTESIAN_POINT('Ctrl Pts',(7.09999865766138,1.31724253497577,0.641005923298765));
#13524=CARTESIAN_POINT('Ctrl Pts',(7.0999987494091,1.31399834762864,0.648240816253195));
#13525=CARTESIAN_POINT('Ctrl Pts',(7.09999933613984,1.30993159792479,0.655050690394837));
#13526=CARTESIAN_POINT('Ctrl Pts',(7.09999956222935,1.30510592187917,0.661272231165006));
#13527=CARTESIAN_POINT('Ctrl Pts',(7.09999960444598,1.30420484616769,0.662433950108221));
#13528=CARTESIAN_POINT('Ctrl Pts',(7.09999963060969,1.30327718139331,0.663575086117144));
#13529=CARTESIAN_POINT('Ctrl Pts',(7.09999963056866,1.30232317316131,0.664694459428815));
#13530=CARTESIAN_POINT('Ctrl Pts',(7.09999963048683,1.30042028596585,0.666927187690779));
#13531=CARTESIAN_POINT('Ctrl Pts',(7.09999952705857,1.29841262431024,0.669073382394206));
#13532=CARTESIAN_POINT('Ctrl Pts',(7.09999938633452,1.29630755303174,0.671129253595323));
#13533=CARTESIAN_POINT('Ctrl Pts',(7.09999900634735,1.29062337821964,0.676680576924663));
#13534=CARTESIAN_POINT('Ctrl Pts',(7.09999841760642,1.2842958957007,0.681513596217188));
#13535=CARTESIAN_POINT('Ctrl Pts',(7.0999982224057,1.2774887935492,0.68557385059291));
#13536=CARTESIAN_POINT('Ctrl Pts',(7.09999809840912,1.27316474526651,0.688153029745784));
#13537=CARTESIAN_POINT('Ctrl Pts',(7.09999810738417,1.26864620899217,0.690419707112974));
#13538=CARTESIAN_POINT('Ctrl Pts',(7.09999825155258,1.26396949224645,0.69235064530212));
#13539=CARTESIAN_POINT('Ctrl Pts',(7.09999847710269,1.25665281355793,0.695371579659609));
#13540=CARTESIAN_POINT('Ctrl Pts',(7.09999903441007,1.2490339950321,0.697538299034574));
#13541=CARTESIAN_POINT('Ctrl Pts',(7.09999948258254,1.24125996729125,0.698781081437474));
#13542=CARTESIAN_POINT('Ctrl Pts',(7.09999977198436,1.23623998534067,0.699583592753232));
#13543=CARTESIAN_POINT('Ctrl Pts',(7.1,1.23115469319345,0.7));
#13544=CARTESIAN_POINT('Ctrl Pts',(7.1,1.22604182196307,0.7));
#13545=CARTESIAN_POINT('Ctrl Pts',(7.1,1.35793097395724,0.));
#13546=CARTESIAN_POINT('Ctrl Pts',(7.1,1.35259441576718,0.100972845781549));
#13547=CARTESIAN_POINT('Ctrl Pts',(7.1,1.34725763161617,0.201946637598055));
#13548=CARTESIAN_POINT('Ctrl Pts',(7.1,1.33659371676552,0.403704849408333));
#13549=CARTESIAN_POINT('Ctrl Pts',(7.0999999994629,1.33126648576411,0.504491180117376));
#13550=CARTESIAN_POINT('Ctrl Pts',(7.0999999994629,1.32593912634735,0.605276549957215));
#13551=CARTESIAN_POINT('Ctrl Pts',(7.11011156210589,-1.35766432821499,-9.27062925672982E-5));
#13552=CARTESIAN_POINT('Ctrl Pts',(7.10674110347764,-1.34708925835705,0.201697046690488));
#13553=CARTESIAN_POINT('Ctrl Pts',(7.10337058314201,-1.33651419103807,0.403486798779133));
#13554=CARTESIAN_POINT('Ctrl Pts',(7.09999999999996,-1.32593912631822,0.605276549958221));
#13555=CARTESIAN_POINT('Ctrl Pts',(5.9694837631095,-1.38835096090528,2.80675674898241E-6));
#13556=CARTESIAN_POINT('Ctrl Pts',(5.96835662351021,-1.37777563343505,0.201792740207853));
#13557=CARTESIAN_POINT('Ctrl Pts',(5.96722945517891,-1.3672003004237,0.40358267322573));
#13558=CARTESIAN_POINT('Ctrl Pts',(5.96610224583462,-1.35662497356325,0.605372606931572));
#13559=CARTESIAN_POINT('Ctrl Pts',(4.8294200007394,-1.39866452387306,3.01102374082134E-5));
#13560=CARTESIAN_POINT('Ctrl Pts',(4.83053730380309,-1.38808904115766,0.201820093264151));
#13561=CARTESIAN_POINT('Ctrl Pts',(4.83165461298617,-1.3775135517806,0.403610075973038));
#13562=CARTESIAN_POINT('Ctrl Pts',(4.83277191472125,-1.36693806692183,0.605400059795761));
#13563=CARTESIAN_POINT('Ctrl Pts',(3.68991216363982,-1.37907703205181,-6.2684699445455E-5));
#13564=CARTESIAN_POINT('Ctrl Pts',(3.69327498756969,-1.36850179198701,0.201727122618256));
#13565=CARTESIAN_POINT('Ctrl Pts',(3.69663785098144,-1.3579265529724,0.403516929334346));
#13566=CARTESIAN_POINT('Ctrl Pts',(3.70000075457889,-1.34735131503281,0.605306735438421));
#13567=CARTESIAN_POINT('Ctrl Pts',(3.69999999992215,-1.34735368792773,0.6052614572053));
#13568=CARTESIAN_POINT('Ctrl Pts',(4.83355316856959,-1.366961322855,0.605214762857233));
#13569=CARTESIAN_POINT('Ctrl Pts',(5.96724522208681,-1.35660163688233,0.605228569880684));
#13570=CARTESIAN_POINT('Ctrl Pts',(7.09999999927392,-1.32593912632169,0.605276549957417));
#13571=CARTESIAN_POINT('Ctrl Pts',(7.1,-1.22604182196307,0.7));
#13572=CARTESIAN_POINT('Ctrl Pts',(5.96696284938742,-1.25674179781664,0.7));
#13573=CARTESIAN_POINT('Ctrl Pts',(4.83327074934872,-1.26710800714677,0.7));
#13574=CARTESIAN_POINT('Ctrl Pts',(3.7,-1.24747724070879,0.7));
#13575=CARTESIAN_POINT('Ctrl Pts',(7.10078315634008,-1.25494559805327,0.7));
#13576=CARTESIAN_POINT('Ctrl Pts',(5.96739926106349,-1.28566432005869,0.700000343763215));
#13577=CARTESIAN_POINT('Ctrl Pts',(4.83328164159484,-1.29603890521481,0.700000334703603));
#13578=CARTESIAN_POINT('Ctrl Pts',(3.69949916377151,-1.27639017438114,0.7));
#13579=CARTESIAN_POINT('Ctrl Pts',(7.10214055788579,-1.30504291366416,0.676629771601708));
#13580=CARTESIAN_POINT('Ctrl Pts',(5.96815960929481,-1.33579288254824,0.676614006760374));
#13581=CARTESIAN_POINT('Ctrl Pts',(4.83329467960724,-1.3461818279488,0.676609489640654));
#13582=CARTESIAN_POINT('Ctrl Pts',(3.69863109538965,-1.3265031696486,0.676624836591801));
#13583=CARTESIAN_POINT('Ctrl Pts',(7.10267376869946,-1.32472200604796,0.626932241521275));
#13584=CARTESIAN_POINT('Ctrl Pts',(5.9684558952243,-1.35546668061705,0.626891484245174));
#13585=CARTESIAN_POINT('Ctrl Pts',(4.83330292199863,-1.36585610284781,0.626879766983475));
#13586=CARTESIAN_POINT('Ctrl Pts',(3.69829020046733,-1.34618280086838,0.626919440930842));
#13587=CARTESIAN_POINT('Ctrl Pts',(7.10270476209941,-1.32586587253612,0.605276664588022));
#13588=CARTESIAN_POINT('Ctrl Pts',(5.96847377630401,-1.35660073810322,0.605228567467576));
#13589=CARTESIAN_POINT('Ctrl Pts',(4.8333022084086,-1.36698748587873,0.605214711607465));
#13590=CARTESIAN_POINT('Ctrl Pts',(3.69827043673666,-1.34732374755196,0.60526152849799));
#13591=CARTESIAN_POINT('Ctrl Pts',(7.1,-1.22604182196307,0.7));
#13592=CARTESIAN_POINT('Ctrl Pts',(5.96696284938742,-1.25674179781664,0.7));
#13593=CARTESIAN_POINT('Ctrl Pts',(4.83327074934872,-1.26710800714677,0.7));
#13594=CARTESIAN_POINT('Ctrl Pts',(3.7,-1.24747724070879,0.7));
#13595=CARTESIAN_POINT('Origin',(5.4,-8.11656130105013E-18,0.7));
#13596=CARTESIAN_POINT('Ctrl Pts',(3.7,1.24747724070879,0.7));
#13597=CARTESIAN_POINT('Ctrl Pts',(4.83327074934871,1.26710800714677,0.7));
#13598=CARTESIAN_POINT('Ctrl Pts',(5.96696284938742,1.25674179781664,0.7));
#13599=CARTESIAN_POINT('Ctrl Pts',(7.1,1.22604182196307,0.7));
#13600=CARTESIAN_POINT('Ctrl Pts',(3.7,1.24747724070879,0.7));
#13601=CARTESIAN_POINT('Ctrl Pts',(4.83327074934871,1.26710800714677,0.7));
#13602=CARTESIAN_POINT('Ctrl Pts',(5.96696284938742,1.25674179781664,0.7));
#13603=CARTESIAN_POINT('Ctrl Pts',(7.1,1.22604182196307,0.7));
#13604=CARTESIAN_POINT('Ctrl Pts',(3.69949916377151,1.27639017438114,0.7));
#13605=CARTESIAN_POINT('Ctrl Pts',(4.83328164159484,1.29603890521481,0.700000334703603));
#13606=CARTESIAN_POINT('Ctrl Pts',(5.96739926106349,1.28566432005869,0.700000343763215));
#13607=CARTESIAN_POINT('Ctrl Pts',(7.10078315634008,1.25494559805327,0.7));
#13608=CARTESIAN_POINT('Ctrl Pts',(3.69863109538965,1.3265031696486,0.676624836591801));
#13609=CARTESIAN_POINT('Ctrl Pts',(4.83329467960724,1.3461818279488,0.676609489640654));
#13610=CARTESIAN_POINT('Ctrl Pts',(5.9681596092948,1.33579288254824,0.676614006760374));
#13611=CARTESIAN_POINT('Ctrl Pts',(7.10214055788579,1.30504291366416,0.676629771601707));
#13612=CARTESIAN_POINT('Ctrl Pts',(3.69829020046733,1.34618280086838,0.626919440930842));
#13613=CARTESIAN_POINT('Ctrl Pts',(4.83330292199863,1.36585610284781,0.626879766983475));
#13614=CARTESIAN_POINT('Ctrl Pts',(5.9684558952243,1.35546668061705,0.626891484245174));
#13615=CARTESIAN_POINT('Ctrl Pts',(7.10267376869946,1.32472200604796,0.626932241521275));
#13616=CARTESIAN_POINT('Ctrl Pts',(3.69827043673666,1.34732374755196,0.60526152849799));
#13617=CARTESIAN_POINT('Ctrl Pts',(4.83330220840859,1.36698748587873,0.605214711607465));
#13618=CARTESIAN_POINT('Ctrl Pts',(5.96847377630401,1.35660073810322,0.605228567467576));
#13619=CARTESIAN_POINT('Ctrl Pts',(7.10270476209941,1.32586587253612,0.605276664588022));
#13620=CARTESIAN_POINT('Ctrl Pts',(7.09999999927392,1.32593912632169,0.605276549957417));
#13621=CARTESIAN_POINT('Ctrl Pts',(5.96724522208681,1.35660163688233,0.605228569880684));
#13622=CARTESIAN_POINT('Ctrl Pts',(4.83355316856959,1.366961322855,0.605214762857233));
#13623=CARTESIAN_POINT('Ctrl Pts',(3.69999999992215,1.34735368792773,0.6052614572053));
#13624=CARTESIAN_POINT('Ctrl Pts',(3.68991216360307,1.37907703216746,-6.26869063400631E-5));
#13625=CARTESIAN_POINT('Ctrl Pts',(3.6932749875452,1.36850179206412,0.201727121146993));
#13626=CARTESIAN_POINT('Ctrl Pts',(3.69663785096921,1.35792655301095,0.403516928598715));
#13627=CARTESIAN_POINT('Ctrl Pts',(3.70000075457892,1.34735131503281,0.605306735438421));
#13628=CARTESIAN_POINT('Ctrl Pts',(4.8294200007272,1.39866452398872,3.01080305115927E-5));
#13629=CARTESIAN_POINT('Ctrl Pts',(4.83053730379496,1.38808904123477,0.201820091792887));
#13630=CARTESIAN_POINT('Ctrl Pts',(4.83165461298211,1.37751355181915,0.403610075237406));
#13631=CARTESIAN_POINT('Ctrl Pts',(4.83277191472127,1.36693806692183,0.605400059795761));
#13632=CARTESIAN_POINT('Ctrl Pts',(5.96948376312183,1.38835096102094,2.80454985295556E-6));
#13633=CARTESIAN_POINT('Ctrl Pts',(5.96835662351844,1.37777563351215,0.201792738736588));
#13634=CARTESIAN_POINT('Ctrl Pts',(5.96722945518303,1.36720030046225,0.403582672490098));
#13635=CARTESIAN_POINT('Ctrl Pts',(5.96610224583462,1.35662497356325,0.605372606931572));
#13636=CARTESIAN_POINT('Ctrl Pts',(7.11011156214274,1.35766432833065,-9.27084994613511E-5));
#13637=CARTESIAN_POINT('Ctrl Pts',(7.10674110350221,1.34708925843416,0.201697045219225));
#13638=CARTESIAN_POINT('Ctrl Pts',(7.10337058315429,1.33651419107662,0.403486798043502));
#13639=CARTESIAN_POINT('Ctrl Pts',(7.09999999999996,1.32593912631822,0.605276549958221));
#13640=CARTESIAN_POINT('Origin',(3.5,1.44777777777778,0.));
#13641=CARTESIAN_POINT('',(3.5,-1.34358136363184,0.605270327458634));
#13642=CARTESIAN_POINT('Ctrl Pts',(3.5,-1.34358136363184,0.605270327458634));
#13643=CARTESIAN_POINT('Ctrl Pts',(3.5,-1.34890136370362,0.504489156176152));
#13644=CARTESIAN_POINT('Ctrl Pts',(3.5,-1.35422123464986,0.403706701640381));
#13645=CARTESIAN_POINT('Ctrl Pts',(3.5,-1.3648706701715,0.201950780690867));
#13646=CARTESIAN_POINT('Ctrl Pts',(3.5,-1.3702003690246,0.100974756199658));
#13647=CARTESIAN_POINT('Ctrl Pts',(3.5,-1.37552980833516,0.));
#13648=CARTESIAN_POINT('',(3.5,-1.24369946473884,0.7));
#13649=CARTESIAN_POINT('Ctrl Pts',(3.49999999991873,-1.24369946470729,0.7));
#13650=CARTESIAN_POINT('Ctrl Pts',(3.49999999896975,-1.25160831520001,0.699999999810925));
#13651=CARTESIAN_POINT('Ctrl Pts',(3.50000040534574,-1.25945374057332,0.69900619751828));
#13652=CARTESIAN_POINT('Ctrl Pts',(3.50000075715473,-1.26709539726361,0.697119355224275));
#13653=CARTESIAN_POINT('Ctrl Pts',(3.5000009551612,-1.27139630362835,0.696057395447694));
#13654=CARTESIAN_POINT('Ctrl Pts',(3.50000113454144,-1.27563271975905,0.694711510656402));
#13655=CARTESIAN_POINT('Ctrl Pts',(3.50000124621709,-1.27977793997275,0.693092697679401));
#13656=CARTESIAN_POINT('Ctrl Pts',(3.50000144618968,-1.28720060051191,0.690193961644836));
#13657=CARTESIAN_POINT('Ctrl Pts',(3.50000138985083,-1.29425038514255,0.686454755369034));
#13658=CARTESIAN_POINT('Ctrl Pts',(3.5000011147959,-1.30078112659466,0.681956784255818));
#13659=CARTESIAN_POINT('Ctrl Pts',(3.50000096334461,-1.30437709646577,0.679480102439082));
#13660=CARTESIAN_POINT('Ctrl Pts',(3.50000075087427,-1.30781543681835,0.676772489296601));
#13661=CARTESIAN_POINT('Ctrl Pts',(3.50000056308077,-1.31106783354026,0.67384203444854));
#13662=CARTESIAN_POINT('Ctrl Pts',(3.50000037990614,-1.31424023611357,0.670983655445047));
#13663=CARTESIAN_POINT('Ctrl Pts',(3.50000021841608,-1.31721646102264,0.667930553458483));
#13664=CARTESIAN_POINT('Ctrl Pts',(3.50000022028926,-1.3199739184757,0.664694242102541));
#13665=CARTESIAN_POINT('Ctrl Pts',(3.50000022375892,-1.32508151834405,0.658699667848218));
#13666=CARTESIAN_POINT('Ctrl Pts',(3.50000072745304,-1.32944146850927,0.652077914129702));
#13667=CARTESIAN_POINT('Ctrl Pts',(3.50000090782832,-1.33299465793893,0.64499486611401));
#13668=CARTESIAN_POINT('Ctrl Pts',(3.50000092626355,-1.33335781125732,0.644270944003422));
#13669=CARTESIAN_POINT('Ctrl Pts',(3.50000094214549,-1.33371249714824,0.643542183465449));
#13670=CARTESIAN_POINT('Ctrl Pts',(3.5000009551778,-1.33405862411533,0.642808750463418));
#13671=CARTESIAN_POINT('Ctrl Pts',(3.50000108270827,-1.3374457225345,0.635631587173848));
#13672=CARTESIAN_POINT('Ctrl Pts',(3.5000008470667,-1.33997810357527,0.628091493562486));
#13673=CARTESIAN_POINT('Ctrl Pts',(3.50000049017339,-1.34160279315579,0.620357239364781));
#13674=CARTESIAN_POINT('Ctrl Pts',(3.50000026118253,-1.3426452308862,0.615394766232079));
#13675=CARTESIAN_POINT('Ctrl Pts',(3.5,-1.34331313055125,0.610351689051435));
#13676=CARTESIAN_POINT('Ctrl Pts',(3.5,-1.34358136363184,0.605270327458634));
#13677=CARTESIAN_POINT('',(3.5,0.723888888888889,0.7));
#13678=CARTESIAN_POINT('Ctrl Pts',(3.5,1.37552980833516,0.));
#13679=CARTESIAN_POINT('Ctrl Pts',(3.5,1.37020035376703,0.10097504527886));
#13680=CARTESIAN_POINT('Ctrl Pts',(3.5,1.36487063968137,0.201951358354439));
#13681=CARTESIAN_POINT('Ctrl Pts',(3.5,1.35422120417274,0.403707279015233));
#13682=CARTESIAN_POINT('Ctrl Pts',(3.5,1.34890134846466,0.504489444860456));
#13683=CARTESIAN_POINT('Ctrl Pts',(3.5,1.34358136363184,0.605270327458635));
#13684=CARTESIAN_POINT('Ctrl Pts',(3.50000000097418,-1.37552980835478,3.46944695195361E-18));
#13685=CARTESIAN_POINT('Ctrl Pts',(3.50374047168104,-1.36494504174376,0.201972406882836));
#13686=CARTESIAN_POINT('Ctrl Pts',(3.50748098869546,-1.35436027657305,0.403944812985359));
#13687=CARTESIAN_POINT('Ctrl Pts',(3.51122155284351,-1.34377551287676,0.605917218294091));
#13688=CARTESIAN_POINT('Ctrl Pts',(2.69119625874569,-1.35924722858667,-7.54309614812119E-5));
#13689=CARTESIAN_POINT('Ctrl Pts',(2.69653217397324,-1.34866266892899,0.20189683354744));
#13690=CARTESIAN_POINT('Ctrl Pts',(2.70186816749714,-1.3380781117335,0.403869096002786));
#13691=CARTESIAN_POINT('Ctrl Pts',(2.7072042346663,-1.32749355863083,0.605841357314298));
#13692=CARTESIAN_POINT('Ctrl Pts',(1.88267190563219,-1.32763345268679,-0.000212792412547521));
#13693=CARTESIAN_POINT('Ctrl Pts',(1.88960380459144,-1.31704931403188,0.201759213581099));
#13694=CARTESIAN_POINT('Ctrl Pts',(1.89653581411498,-1.30646518166523,0.403731216009517));
#13695=CARTESIAN_POINT('Ctrl Pts',(1.90346792975642,-1.29588105699583,0.605703215867581));
#13696=CARTESIAN_POINT('Ctrl Pts',(1.07441451989529,-1.27728918272486,-0.000429194541766893));
#13697=CARTESIAN_POINT('Ctrl Pts',(1.08294287068452,-1.26670581246828,0.201542410257184));
#13698=CARTESIAN_POINT('Ctrl Pts',(1.09147136321593,-1.25612245578053,0.403514009799157));
#13699=CARTESIAN_POINT('Ctrl Pts',(1.09999999999989,-1.24553911298205,0.605485603995245));
#13700=CARTESIAN_POINT('Ctrl Pts',(1.09999999916631,-1.24553911263844,0.605485603997431));
#13701=CARTESIAN_POINT('Ctrl Pts',(1.89930203168262,-1.29563783986497,0.605377360150118));
#13702=CARTESIAN_POINT('Ctrl Pts',(2.69958486793449,-1.32722445934619,0.605308375488923));
#13703=CARTESIAN_POINT('Ctrl Pts',(3.5,-1.34358136363184,0.605270327458634));
#13704=CARTESIAN_POINT('Ctrl Pts',(3.50204003610941,-1.24374118183538,0.7));
#13705=CARTESIAN_POINT('Ctrl Pts',(2.70080437300401,-1.2273695200909,0.7));
#13706=CARTESIAN_POINT('Ctrl Pts',(1.89984199608574,-1.1957170361627,0.7));
#13707=CARTESIAN_POINT('Ctrl Pts',(1.1,-1.14549341399196,0.7));
#13708=CARTESIAN_POINT('Ctrl Pts',(3.50144932661635,-1.27265074030048,0.7));
#13709=CARTESIAN_POINT('Ctrl Pts',(2.6998452019678,-1.25626413437997,0.699999727319846));
#13710=CARTESIAN_POINT('Ctrl Pts',(1.89847848223078,-1.22458382597074,0.70000077422621));
#13711=CARTESIAN_POINT('Ctrl Pts',(1.09819048660397,-1.17431102498992,0.7));
#13712=CARTESIAN_POINT('Ctrl Pts',(3.50042536655637,-1.322763754511,0.676632802377821));
#13713=CARTESIAN_POINT('Ctrl Pts',(2.69818680938114,-1.3063522351595,0.67664530655333));
#13714=CARTESIAN_POINT('Ctrl Pts',(1.89610976425884,-1.27462253270773,0.67666760713801));
#13715=CARTESIAN_POINT('Ctrl Pts',(1.09505363188407,-1.22426736091617,0.676703190608825));
#13716=CARTESIAN_POINT('Ctrl Pts',(3.50002334924346,-1.34243864233338,0.626926882269943));
#13717=CARTESIAN_POINT('Ctrl Pts',(2.6975332861013,-1.32603127467068,0.626959208652505));
#13718=CARTESIAN_POINT('Ctrl Pts',(1.89518106151152,-1.29430885982199,0.62701751976321));
#13719=CARTESIAN_POINT('Ctrl Pts',(1.09381704710221,-1.24396073223232,0.627109609335854));
#13720=CARTESIAN_POINT('Ctrl Pts',(3.5,-1.34358136363184,0.605270327458634));
#13721=CARTESIAN_POINT('Ctrl Pts',(2.69749615303,-1.32718177535833,0.605308474776761));
#13722=CARTESIAN_POINT('Ctrl Pts',(1.89512529323683,-1.29547288309274,0.605377720397184));
#13723=CARTESIAN_POINT('Ctrl Pts',(1.09374258853658,-1.24514653057163,0.605486452199395));
#13724=CARTESIAN_POINT('Ctrl Pts',(3.49999999991875,-1.24369946470729,0.7));
#13725=CARTESIAN_POINT('Ctrl Pts',(3.26917843083003,-1.23897560807887,0.7));
#13726=CARTESIAN_POINT('Ctrl Pts',(3.03837960179139,-1.23298334389983,0.7));
#13727=CARTESIAN_POINT('Ctrl Pts',(2.80762376541487,-1.22564400623233,0.7));
#13728=CARTESIAN_POINT('Ctrl Pts',(2.57739190516312,-1.2178709162388,0.7));
#13729=CARTESIAN_POINT('Ctrl Pts',(2.08463535466707,-1.20026407570248,0.7));
#13730=CARTESIAN_POINT('Ctrl Pts',(1.59210562457525,-1.17639367564078,0.7));
#13731=CARTESIAN_POINT('Ctrl Pts',(1.1,-1.14549341399196,0.7));
#13732=CARTESIAN_POINT('Origin',(5.4,-8.11656130105013E-18,0.7));
#13733=CARTESIAN_POINT('Ctrl Pts',(1.0744145198953,1.27728918272486,-0.000429194541767127));
#13734=CARTESIAN_POINT('Ctrl Pts',(1.08294287068452,1.26670581246828,0.201542410257184));
#13735=CARTESIAN_POINT('Ctrl Pts',(1.09147136321593,1.25612245578053,0.403514009799157));
#13736=CARTESIAN_POINT('Ctrl Pts',(1.0999999999999,1.24553911298205,0.605485603995245));
#13737=CARTESIAN_POINT('Ctrl Pts',(1.88267190563235,1.3276334526868,-0.000212792412547728));
#13738=CARTESIAN_POINT('Ctrl Pts',(1.8896038045916,1.31704931403189,0.201759213581098));
#13739=CARTESIAN_POINT('Ctrl Pts',(1.89653581411514,1.30646518166524,0.403731216009517));
#13740=CARTESIAN_POINT('Ctrl Pts',(1.90346792975658,1.29588105699584,0.605703215867581));
#13741=CARTESIAN_POINT('Ctrl Pts',(2.69119625874601,1.35924722858668,-7.54309614812134E-5));
#13742=CARTESIAN_POINT('Ctrl Pts',(2.69653217397356,1.348662668929,0.201896833547441));
#13743=CARTESIAN_POINT('Ctrl Pts',(2.70186816749745,1.33807811173351,0.403869096002786));
#13744=CARTESIAN_POINT('Ctrl Pts',(2.70720423466661,1.32749355863085,0.605841357314298));
#13745=CARTESIAN_POINT('Ctrl Pts',(3.50000000097466,1.37552980835479,-3.81639164714898E-17));
#13746=CARTESIAN_POINT('Ctrl Pts',(3.50374047168151,1.36494504174377,0.201972406882836));
#13747=CARTESIAN_POINT('Ctrl Pts',(3.50748098869594,1.35436027657306,0.403944812985359));
#13748=CARTESIAN_POINT('Ctrl Pts',(3.51122155284398,1.34377551287677,0.605917218294091));
#13749=CARTESIAN_POINT('Origin',(0.9,1.34328341716202,0.));
#13750=CARTESIAN_POINT('',(0.9,-1.23261418131727,0.605513513251856));
#13751=CARTESIAN_POINT('Ctrl Pts',(0.9,-1.23261418131727,0.605513513251856));
#13752=CARTESIAN_POINT('Ctrl Pts',(0.9,-1.23820195798151,0.504544236118289));
#13753=CARTESIAN_POINT('Ctrl Pts',(0.9,-1.24378834611607,0.403573587101897));
#13754=CARTESIAN_POINT('Ctrl Pts',(0.9,-1.25495246062481,0.201736610752668));
#13755=CARTESIAN_POINT('Ctrl Pts',(0.9,-1.26053033259331,0.100867703930409));
#13756=CARTESIAN_POINT('Ctrl Pts',(0.9,-1.266106713614,0.));
#13757=CARTESIAN_POINT('',(0.9,-1.13254484134404,0.7));
#13758=CARTESIAN_POINT('Ctrl Pts',(0.899999999937205,-1.13254484130906,
0.7));
#13759=CARTESIAN_POINT('Ctrl Pts',(0.899999996287105,-1.14047016437301,
0.699999998205918));
#13760=CARTESIAN_POINT('Ctrl Pts',(0.900001280561548,-1.14833327216777,
0.699006663725481));
#13761=CARTESIAN_POINT('Ctrl Pts',(0.900002371513522,-1.15599299513142,
0.697119896446058));
#13762=CARTESIAN_POINT('Ctrl Pts',(0.900002982478546,-1.16028266409831,
0.696063251566776));
#13763=CARTESIAN_POINT('Ctrl Pts',(0.900003528700818,-1.16450859688491,
0.694725368779139));
#13764=CARTESIAN_POINT('Ctrl Pts',(0.900003857331964,-1.16864431737637,
0.693116947675672));
#13765=CARTESIAN_POINT('Ctrl Pts',(0.900004447924614,-1.17607674172948,
0.690226407030055));
#13766=CARTESIAN_POINT('Ctrl Pts',(0.900004211500339,-1.18313828052408,
0.686496282267003));
#13767=CARTESIAN_POINT('Ctrl Pts',(0.900003280035406,-1.18968205680082,
0.682006679400108));
#13768=CARTESIAN_POINT('Ctrl Pts',(0.900002768383153,-1.19327654302499,
0.679540547464272));
#13769=CARTESIAN_POINT('Ctrl Pts',(0.900002064672634,-1.19671453445753,
0.676844382327844));
#13770=CARTESIAN_POINT('Ctrl Pts',(0.900001450170085,-1.19996775918788,
0.673925988054463));
#13771=CARTESIAN_POINT('Ctrl Pts',(0.900000850201302,-1.20314404102283,
0.67107661751105));
#13772=CARTESIAN_POINT('Ctrl Pts',(0.900000329673364,-1.20612495630093,
0.668032594545539));
#13773=CARTESIAN_POINT('Ctrl Pts',(0.900000346081477,-1.20888784276431,
0.664805176146368));
#13774=CARTESIAN_POINT('Ctrl Pts',(0.900000376514472,-1.21401231436848,
0.658819112599938));
#13775=CARTESIAN_POINT('Ctrl Pts',(0.900002057232535,-1.21838968018573,
0.652203523053766));
#13776=CARTESIAN_POINT('Ctrl Pts',(0.900002698394847,-1.22195969054856,
0.645123732731769));
#13777=CARTESIAN_POINT('Ctrl Pts',(0.900002763240662,-1.22232075393107,
0.644407697543824));
#13778=CARTESIAN_POINT('Ctrl Pts',(0.90000282009371,-1.22267351953901,0.643686895083047));
#13779=CARTESIAN_POINT('Ctrl Pts',(0.900002868017411,-1.22301789747605,
0.642961485862499));
#13780=CARTESIAN_POINT('Ctrl Pts',(0.900003341628975,-1.22642125256928,
0.635792544708285));
#13781=CARTESIAN_POINT('Ctrl Pts',(0.900002645022176,-1.22896979279554,
0.628258742918086));
#13782=CARTESIAN_POINT('Ctrl Pts',(0.900001532827652,-1.23061007098772,
0.6205286650049));
#13783=CARTESIAN_POINT('Ctrl Pts',(0.900000822323555,-1.23165793118585,
0.61559045329652));
#13784=CARTESIAN_POINT('Ctrl Pts',(0.900000000000001,-1.23233426661673,
0.610571479357261));
#13785=CARTESIAN_POINT('Ctrl Pts',(0.900000000000001,-1.23261418131727,
0.605513513251856));
#13786=CARTESIAN_POINT('',(0.9,1.13254484134404,0.7));
#13787=CARTESIAN_POINT('',(0.9,0.671641708581009,0.7));
#13788=CARTESIAN_POINT('',(0.9,1.23261418131727,0.605513513251856));
#13789=CARTESIAN_POINT('Ctrl Pts',(0.9,1.23261418131727,0.605513513251856));
#13790=CARTESIAN_POINT('Ctrl Pts',(0.9,1.23217633603244,0.613425232807268));
#13791=CARTESIAN_POINT('Ctrl Pts',(0.900001832787994,1.23077105609892,0.621244170085157));
#13792=CARTESIAN_POINT('Ctrl Pts',(0.900002580745575,1.22848219166492,0.628809599741497));
#13793=CARTESIAN_POINT('Ctrl Pts',(0.900002993068559,1.22722042035689,0.632980157827643));
#13794=CARTESIAN_POINT('Ctrl Pts',(0.90000314174678,1.22568915198244,0.637073706995481));
#13795=CARTESIAN_POINT('Ctrl Pts',(0.900002971484041,1.2238959908032,0.641061424759933));
#13796=CARTESIAN_POINT('Ctrl Pts',(0.900002662567364,1.22064256379503,0.648296551655426));
#13797=CARTESIAN_POINT('Ctrl Pts',(0.900001146653719,1.21656554418039,0.655104870690721));
#13798=CARTESIAN_POINT('Ctrl Pts',(0.900000540233788,1.21172928299109,0.66132323772617));
#13799=CARTESIAN_POINT('Ctrl Pts',(0.900000424918953,1.21080963534652,0.66250570210793));
#13800=CARTESIAN_POINT('Ctrl Pts',(0.900000351402035,1.20986240082127,0.663666762843393));
#13801=CARTESIAN_POINT('Ctrl Pts',(0.900000346234225,1.20888784277449,0.664805176146358));
#13802=CARTESIAN_POINT('Ctrl Pts',(0.900000336405833,1.20703438079614,0.666970266034709));
#13803=CARTESIAN_POINT('Ctrl Pts',(0.900000571869483,1.20508211779724,0.669053482241208));
#13804=CARTESIAN_POINT('Ctrl Pts',(0.900000903580486,1.20303784749416,0.671051418948595));
#13805=CARTESIAN_POINT('Ctrl Pts',(0.900001825932764,1.19735357006848,0.676606861644505));
#13806=CARTESIAN_POINT('Ctrl Pts',(0.900003332967427,1.19102482074992,0.681443262092019));
#13807=CARTESIAN_POINT('Ctrl Pts',(0.900003895332687,1.18421635668109,0.685507797106414));
#13808=CARTESIAN_POINT('Ctrl Pts',(0.900004254598985,1.17986677848026,0.688104419886002));
#13809=CARTESIAN_POINT('Ctrl Pts',(0.9000042929279,1.17532044218795,0.69038534615497));
#13810=CARTESIAN_POINT('Ctrl Pts',(0.900003997675654,1.17061445353731,0.692327416690341));
#13811=CARTESIAN_POINT('Ctrl Pts',(0.900003537640084,1.16328200409216,0.695353376818313));
#13812=CARTESIAN_POINT('Ctrl Pts',(0.900002259964378,1.15564663185935,0.697524398440697));
#13813=CARTESIAN_POINT('Ctrl Pts',(0.900001215101098,1.14785635641255,0.698771715080855));
#13814=CARTESIAN_POINT('Ctrl Pts',(0.900000537649455,1.14280542295857,0.699580430175527));
#13815=CARTESIAN_POINT('Ctrl Pts',(0.899999997568109,1.13768876957788,0.699999998835552));
#13816=CARTESIAN_POINT('Ctrl Pts',(0.899999999937205,1.13254484130906,0.7));
#13817=CARTESIAN_POINT('Ctrl Pts',(0.9,1.266106713614,0.));
#13818=CARTESIAN_POINT('Ctrl Pts',(0.9,1.26053025554556,0.100869097599589));
#13819=CARTESIAN_POINT('Ctrl Pts',(0.9,1.25495230648558,0.201739398169819));
#13820=CARTESIAN_POINT('Ctrl Pts',(0.9,1.24378819189631,0.403576374532447));
#13821=CARTESIAN_POINT('Ctrl Pts',(0.9,1.23820188085298,0.504545629805417));
#13822=CARTESIAN_POINT('Ctrl Pts',(0.9,1.23261418131727,0.605513513251856));
#13823=CARTESIAN_POINT('Ctrl Pts',(0.900000000000002,-1.266106713614,-8.15320033709099E-17));
#13824=CARTESIAN_POINT('Ctrl Pts',(0.908871090277923,-1.25552568177643,
0.201930159665972));
#13825=CARTESIAN_POINT('Ctrl Pts',(0.917742329685194,-1.24494466498547,
0.403860313587921));
#13826=CARTESIAN_POINT('Ctrl Pts',(0.926613720860141,-1.23436366359623,
0.605790461668883));
#13827=CARTESIAN_POINT('Ctrl Pts',(0.697441255022372,-1.25280938151844,
-5.71013218131409E-5));
#13828=CARTESIAN_POINT('Ctrl Pts',(0.706712389899261,-1.24222855501813,
0.201872952723963));
#13829=CARTESIAN_POINT('Ctrl Pts',(0.71598368260269,-1.23164774534186,0.403803000441224));
#13830=CARTESIAN_POINT('Ctrl Pts',(0.725255135891715,-1.22106695288555,
0.605733041729342));
#13831=CARTESIAN_POINT('Ctrl Pts',(0.494899146035781,-1.23832021354117,
-0.000119230777047918));
#13832=CARTESIAN_POINT('Ctrl Pts',(0.504570354086872,-1.2277396148863,0.201810708652083));
#13833=CARTESIAN_POINT('Ctrl Pts',(0.514241728780064,-1.21715903502506,
0.403740641123913));
#13834=CARTESIAN_POINT('Ctrl Pts',(0.523913273026478,-1.20657847439907,
0.605670566527588));
#13835=CARTESIAN_POINT('Ctrl Pts',(0.292373353339556,-1.22258574808743,
-0.000186633859775947));
#13836=CARTESIAN_POINT('Ctrl Pts',(0.302444661323169,-1.21200540195431,
0.201743181663441));
#13837=CARTESIAN_POINT('Ctrl Pts',(0.312516144861689,-1.20142507679253,
0.403672989556125));
#13838=CARTESIAN_POINT('Ctrl Pts',(0.322587807049886,-1.190844773096,0.605602789690272));
#13839=CARTESIAN_POINT('',(0.32407846024449,-1.19096124572524,0.605603291426262));
#13840=CARTESIAN_POINT('Ctrl Pts',(0.292382661757373,-1.22257596919059,
-1.26634813746307E-16));
#13841=CARTESIAN_POINT('Ctrl Pts',(0.302948004341657,-1.21203750712027,
0.201867748891544));
#13842=CARTESIAN_POINT('Ctrl Pts',(0.313513270922098,-1.20149926476964,
0.403735512620674));
#13843=CARTESIAN_POINT('Ctrl Pts',(0.324078460244491,-1.19096124572524,
0.605603291426262));
#13844=CARTESIAN_POINT('Ctrl Pts',(0.324078460244487,-1.19096124572524,
0.605603291426262));
#13845=CARTESIAN_POINT('Ctrl Pts',(0.515976798438381,-1.20595780001216,
0.605571001180369));
#13846=CARTESIAN_POINT('Ctrl Pts',(0.707956283694857,-1.21982772882273,
0.605541108414459));
#13847=CARTESIAN_POINT('Ctrl Pts',(0.900000000000001,-1.23261418131727,
0.605513513251856));
#13848=CARTESIAN_POINT('Ctrl Pts',(0.906632491847682,-1.13298681949577,
0.7));
#13849=CARTESIAN_POINT('Ctrl Pts',(0.714963137593258,-1.12022681655782,
0.7));
#13850=CARTESIAN_POINT('Ctrl Pts',(0.52336552158394,-1.10638609587519,0.7));
#13851=CARTESIAN_POINT('Ctrl Pts',(0.331856371369197,-1.09142177001972,
0.7));
#13852=CARTESIAN_POINT('Ctrl Pts',(0.904714827274509,-1.16179226195561,
0.7));
#13853=CARTESIAN_POINT('Ctrl Pts',(0.712937153454425,-1.14901967286075,
0.69999980360337));
#13854=CARTESIAN_POINT('Ctrl Pts',(0.521230340369869,-1.13516557394852,
0.700000229443053));
#13855=CARTESIAN_POINT('Ctrl Pts',(0.329608751265076,-1.12018616744754,
0.7));
#13856=CARTESIAN_POINT('Ctrl Pts',(0.901389714107723,-1.21173913866089,
0.676722045797292));
#13857=CARTESIAN_POINT('Ctrl Pts',(0.709425477581998,-1.19894546296063,
0.676731074746188));
#13858=CARTESIAN_POINT('Ctrl Pts',(0.517526696841433,-1.18506766126723,
0.67674067107047));
#13859=CARTESIAN_POINT('Ctrl Pts',(0.325711429829026,-1.17006296935233,
0.676751229163451));
#13860=CARTESIAN_POINT('Ctrl Pts',(0.900079298017777,-1.23142303740181,
0.627132481749528));
#13861=CARTESIAN_POINT('Ctrl Pts',(0.708040181852795,-1.21863106773591,
0.627155851652593));
#13862=CARTESIAN_POINT('Ctrl Pts',(0.516066269599777,-1.20475540724405,
0.627181012790208));
#13863=CARTESIAN_POINT('Ctrl Pts',(0.324172915772929,-1.18975243096407,
0.627208352638976));
#13864=CARTESIAN_POINT('Ctrl Pts',(0.900000000000001,-1.23261418131727,
0.605513513251856));
#13865=CARTESIAN_POINT('Ctrl Pts',(0.707956283694857,-1.21982772882273,
0.605541108414459));
#13866=CARTESIAN_POINT('Ctrl Pts',(0.515976798438381,-1.20595780001216,
0.605571001180369));
#13867=CARTESIAN_POINT('Ctrl Pts',(0.324078460244487,-1.19096124572524,
0.605603291426262));
#13868=CARTESIAN_POINT('',(0.3318563713692,-1.09142177001972,0.7));
#13869=CARTESIAN_POINT('Origin',(0.3318563713692,-1.09142177001972,0.6));
#13870=CARTESIAN_POINT('Ctrl Pts',(0.899999999937167,-1.13254484130906,
0.7));
#13871=CARTESIAN_POINT('Ctrl Pts',(0.710543123935439,-1.11990737114256,
0.7));
#13872=CARTESIAN_POINT('Ctrl Pts',(0.521156529292483,-1.10621348751457,
0.7));
#13873=CARTESIAN_POINT('Ctrl Pts',(0.331856371369197,-1.09142177001972,
0.7));
#13874=CARTESIAN_POINT('Origin',(5.4,-8.11656130105013E-18,0.7));
#13875=CARTESIAN_POINT('',(0.3318563713692,1.09142177001972,0.7));
#13876=CARTESIAN_POINT('',(0.3318563713692,-0.7,0.7));
#13877=CARTESIAN_POINT('Ctrl Pts',(0.3318563713692,1.09142177001972,0.7));
#13878=CARTESIAN_POINT('Ctrl Pts',(0.521156529292483,1.10621348751457,0.7));
#13879=CARTESIAN_POINT('Ctrl Pts',(0.710543123935438,1.11990737114256,0.7));
#13880=CARTESIAN_POINT('Ctrl Pts',(0.899999999937165,1.13254484130906,0.7));
#13881=CARTESIAN_POINT('Ctrl Pts',(0.292373353339556,1.22258574808743,-0.000186633859776018));
#13882=CARTESIAN_POINT('Ctrl Pts',(0.30244466132317,1.21200540195431,0.20174318166344));
#13883=CARTESIAN_POINT('Ctrl Pts',(0.31251614486169,1.20142507679253,0.403672989556124));
#13884=CARTESIAN_POINT('Ctrl Pts',(0.322587807049886,1.190844773096,0.605602789690271));
#13885=CARTESIAN_POINT('Ctrl Pts',(0.494899146035781,1.23832021354117,-0.000119230777047989));
#13886=CARTESIAN_POINT('Ctrl Pts',(0.504570354086872,1.2277396148863,0.201810708652083));
#13887=CARTESIAN_POINT('Ctrl Pts',(0.514241728780064,1.21715903502506,0.403740641123914));
#13888=CARTESIAN_POINT('Ctrl Pts',(0.523913273026478,1.20657847439907,0.605670566527587));
#13889=CARTESIAN_POINT('Ctrl Pts',(0.697441255022371,1.25280938151844,-5.71013218130602E-5));
#13890=CARTESIAN_POINT('Ctrl Pts',(0.70671238989926,1.24222855501813,0.201872952723963));
#13891=CARTESIAN_POINT('Ctrl Pts',(0.715983682602689,1.23164774534186,0.403803000441224));
#13892=CARTESIAN_POINT('Ctrl Pts',(0.725255135891714,1.22106695288555,0.605733041729342));
#13893=CARTESIAN_POINT('Ctrl Pts',(0.9,1.266106713614,1.73472347597681E-18));
#13894=CARTESIAN_POINT('Ctrl Pts',(0.908871090277921,1.25552568177643,0.201930159665973));
#13895=CARTESIAN_POINT('Ctrl Pts',(0.917742329685192,1.24494466498547,0.403860313587921));
#13896=CARTESIAN_POINT('Ctrl Pts',(0.92661372086014,1.23436366359623,0.605790461668883));
#13897=CARTESIAN_POINT('',(0.32407846024449,1.19096124572524,0.605603291426262));
#13898=CARTESIAN_POINT('Ctrl Pts',(0.9,1.23261418131727,0.605513513251856));
#13899=CARTESIAN_POINT('Ctrl Pts',(0.707956283694857,1.21982772882273,0.605541108414459));
#13900=CARTESIAN_POINT('Ctrl Pts',(0.515976798438382,1.20595780001216,0.60557100118037));
#13901=CARTESIAN_POINT('Ctrl Pts',(0.32407846024449,1.19096124572524,0.605603291426262));
#13902=CARTESIAN_POINT('Ctrl Pts',(0.324078460244491,1.19096124572524,0.605603291426262));
#13903=CARTESIAN_POINT('Ctrl Pts',(0.313513270922098,1.20149926476964,0.403735512620674));
#13904=CARTESIAN_POINT('Ctrl Pts',(0.302948004341658,1.21203750712026,0.201867748891544));
#13905=CARTESIAN_POINT('Ctrl Pts',(0.292382661757373,1.22257596919059,3.4477629085039E-17));
#13906=CARTESIAN_POINT('Ctrl Pts',(0.3318563713692,1.09142177001972,0.7));
#13907=CARTESIAN_POINT('Ctrl Pts',(0.523365521583941,1.10638609587519,0.7));
#13908=CARTESIAN_POINT('Ctrl Pts',(0.714963137593258,1.12022681655782,0.7));
#13909=CARTESIAN_POINT('Ctrl Pts',(0.906632491847681,1.13298681949577,0.7));
#13910=CARTESIAN_POINT('Ctrl Pts',(0.329608751265078,1.12018616744754,0.7));
#13911=CARTESIAN_POINT('Ctrl Pts',(0.52123034036987,1.13516557394852,0.700000229443053));
#13912=CARTESIAN_POINT('Ctrl Pts',(0.712937153454426,1.14901967286075,0.699999803603371));
#13913=CARTESIAN_POINT('Ctrl Pts',(0.904714827274509,1.16179226195561,0.700000000000001));
#13914=CARTESIAN_POINT('Ctrl Pts',(0.325711429829028,1.17006296935233,0.676751229163452));
#13915=CARTESIAN_POINT('Ctrl Pts',(0.517526696841433,1.18506766126723,0.67674067107047));
#13916=CARTESIAN_POINT('Ctrl Pts',(0.709425477581997,1.19894546296063,0.676731074746189));
#13917=CARTESIAN_POINT('Ctrl Pts',(0.901389714107722,1.21173913866089,0.676722045797292));
#13918=CARTESIAN_POINT('Ctrl Pts',(0.324172915772932,1.18975243096407,0.627208352638976));
#13919=CARTESIAN_POINT('Ctrl Pts',(0.516066269599778,1.20475540724405,0.627181012790208));
#13920=CARTESIAN_POINT('Ctrl Pts',(0.708040181852794,1.21863106773591,0.627155851652593));
#13921=CARTESIAN_POINT('Ctrl Pts',(0.900079298017776,1.23142303740181,0.627132481749528));
#13922=CARTESIAN_POINT('Ctrl Pts',(0.32407846024449,1.19096124572524,0.605603291426262));
#13923=CARTESIAN_POINT('Ctrl Pts',(0.515976798438382,1.20595780001216,0.60557100118037));
#13924=CARTESIAN_POINT('Ctrl Pts',(0.707956283694857,1.21982772882273,0.605541108414459));
#13925=CARTESIAN_POINT('Ctrl Pts',(0.9,1.23261418131727,0.605513513251856));
#13926=CARTESIAN_POINT('Origin',(0.331856371369202,1.09142177001972,0.6));
#13927=CARTESIAN_POINT('Origin',(0.331856371369202,1.09142177001972,0.6));
#13928=CARTESIAN_POINT('Origin',(0.331856371369201,1.09142177001972,0.6));
#13929=CARTESIAN_POINT('Origin',(0.331856371369202,1.09142177001972,0.6));
#13930=CARTESIAN_POINT('Origin',(10.4681436286308,1.08420482079361,0.6));
#13931=CARTESIAN_POINT('Origin',(10.4681436276939,1.08420482084454,0.6));
#13932=CARTESIAN_POINT('',(10.5680065821063,1.08420482079361,0.605233595624295));
#13933=CARTESIAN_POINT('Origin',(10.4681436286308,1.08420482079361,0.6));
#13934=CARTESIAN_POINT('Origin',(10.4681436286308,1.08420482079361,0.6));
#13935=CARTESIAN_POINT('Origin',(0.3318563713692,-1.09142177001972,0.6));
#13936=CARTESIAN_POINT('Origin',(0.331856371369201,-1.09142177001972,0.6));
#13937=CARTESIAN_POINT('Origin',(0.3318563713692,-1.09142177001972,0.6));
#13938=CARTESIAN_POINT('Origin',(0.3318563713692,-0.7,0.6));
#13939=CARTESIAN_POINT('Ctrl Pts',(0.2922895713475,-1.22266882276207,-0.00177864096060679));
#13940=CARTESIAN_POINT('Ctrl Pts',(0.302885944515497,-1.21209940820877,
0.200681988163859));
#13941=CARTESIAN_POINT('Ctrl Pts',(0.313482241236256,-1.20153021465708,
0.403142632212487));
#13942=CARTESIAN_POINT('Ctrl Pts',(0.324078460244491,-1.19096124572524,
0.605603291426262));
#13943=CARTESIAN_POINT('Ctrl Pts',(0.264022491930188,-1.22039553779506,
-0.000415890128406236));
#13944=CARTESIAN_POINT('Ctrl Pts',(0.274621881512248,-1.20982222712748,
0.202044379074236));
#13945=CARTESIAN_POINT('Ctrl Pts',(0.285221154833576,-1.19924944554801,
0.404504681968985));
#13946=CARTESIAN_POINT('Ctrl Pts',(0.29582042516239,-1.18867654001483,0.606964977361795));
#13947=CARTESIAN_POINT('Ctrl Pts',(0.216712469170969,-1.1940874043406,0.000690255297866666));
#13948=CARTESIAN_POINT('Ctrl Pts',(0.227319688237882,-1.18351239299796,
0.203150045648192));
#13949=CARTESIAN_POINT('Ctrl Pts',(0.237926932441998,-1.17293746916702,
0.405609838636422));
#13950=CARTESIAN_POINT('Ctrl Pts',(0.248534117816369,-1.1623628476683,0.608069650238703));
#13951=CARTESIAN_POINT('Ctrl Pts',(0.200219987929043,-1.14439035743082,
-0.00103956457010847));
#13952=CARTESIAN_POINT('Ctrl Pts',(0.210830491339948,-1.13382006821851,
0.201420337884579));
#13953=CARTESIAN_POINT('Ctrl Pts',(0.221440906577676,-1.12324995278282,
0.403880253819325));
#13954=CARTESIAN_POINT('Ctrl Pts',(0.232051411471599,-1.11268010558856,
0.606340179010355));
#13955=CARTESIAN_POINT('Ctrl Pts',(0.200161975173303,-1.12312592850316,
-0.00214651389202307));
#13956=CARTESIAN_POINT('Ctrl Pts',(0.210772455448684,-1.11255764422181,
0.200313510564959));
#13957=CARTESIAN_POINT('Ctrl Pts',(0.221382936352032,-1.1019895901204,0.402773547004277));
#13958=CARTESIAN_POINT('Ctrl Pts',(0.231993417893744,-1.09142177001972,
0.605233595624295));
#13959=CARTESIAN_POINT('Origin',(10.4681436286308,-1.08420482109828,0.6));
#13960=CARTESIAN_POINT('',(10.5680065821063,-1.08420482079361,0.605233595624295));
#13961=CARTESIAN_POINT('Origin',(10.4681436286308,-1.08420482099672,0.600000000000001));
#13962=CARTESIAN_POINT('Origin',(10.4681436286308,-1.08420482109828,0.6));
#13963=CARTESIAN_POINT('Origin',(10.4681436286308,0.7,0.6));
#13964=CARTESIAN_POINT('',(10.5680065821063,0.7,0.605233595624295));
#13965=CARTESIAN_POINT('Ctrl Pts',(10.599839982685,-1.11594741464673,-0.00218387205330164));
#13966=CARTESIAN_POINT('Ctrl Pts',(10.5892288496247,-1.10536637943871,0.200288608282177));
#13967=CARTESIAN_POINT('Ctrl Pts',(10.5786177161011,-1.0947855138519,0.402761097457634));
#13968=CARTESIAN_POINT('Ctrl Pts',(10.5680065821063,-1.08420482079362,0.605233595624295));
#13969=CARTESIAN_POINT('Ctrl Pts',(10.5997613205547,-1.14474784499259,-0.000682909193257743));
#13970=CARTESIAN_POINT('Ctrl Pts',(10.5891501209488,-1.13416481604349,0.201789447273867));
#13971=CARTESIAN_POINT('Ctrl Pts',(10.5785391399155,-1.12358205581644,0.404261829287571));
#13972=CARTESIAN_POINT('Ctrl Pts',(10.5679279386544,-1.11299934606825,0.606734202078189));
#13973=CARTESIAN_POINT('Ctrl Pts',(10.5764119435127,-1.19466846760808,0.000702210001053139));
#13974=CARTESIAN_POINT('Ctrl Pts',(10.5658041809617,-1.18408222297768,0.203174550667819));
#13975=CARTESIAN_POINT('Ctrl Pts',(10.5551963844732,-1.17349608774572,0.405646894856767));
#13976=CARTESIAN_POINT('Ctrl Pts',(10.544588659013,-1.16291012508165,0.608119251464957));
#13977=CARTESIAN_POINT('Ctrl Pts',(10.5269342003857,-1.21442651155969,-0.000858270497959616));
#13978=CARTESIAN_POINT('Ctrl Pts',(10.5163317654776,-1.20384274018949,0.201614467507756));
#13979=CARTESIAN_POINT('Ctrl Pts',(10.5057293269973,-1.1932591813998,0.404087216090532));
#13980=CARTESIAN_POINT('Ctrl Pts',(10.4951269905998,-1.18267571840064,0.606559974437339));
#13981=CARTESIAN_POINT('Ctrl Pts',(10.5053655128635,-1.21565094114741,-0.0019246498908503));
#13982=CARTESIAN_POINT('Ctrl Pts',(10.4947646468921,-1.20506932615592,0.200548282383137));
#13983=CARTESIAN_POINT('Ctrl Pts',(10.4841638390504,-1.19448787589602,0.403021225840181));
#13984=CARTESIAN_POINT('Ctrl Pts',(10.4735630903435,-1.18390659316268,0.605494180667945));
#13985=CARTESIAN_POINT('Ctrl Pts',(10.5997255308004,-1.11583328740478,1.02782365951626E-16));
#13986=CARTESIAN_POINT('Ctrl Pts',(10.589152548365,-1.10529029582828,0.201744523047832));
#13987=CARTESIAN_POINT('Ctrl Pts',(10.5785795654695,-1.09474747266587,0.40348905487273));
#13988=CARTESIAN_POINT('Ctrl Pts',(10.5680065821063,-1.08420482079362,0.605233595624295));
#13989=CARTESIAN_POINT('Ctrl Pts',(10.5053638082297,1.21564923960921,-0.0018920919656423));
#13990=CARTESIAN_POINT('Ctrl Pts',(10.4947635104759,1.20506819181477,0.200569987667808));
#13991=CARTESIAN_POINT('Ctrl Pts',(10.4841632708454,1.19448730873444,0.403032078483127));
#13992=CARTESIAN_POINT('Ctrl Pts',(10.4735630903435,1.18390659316268,0.605494180667945));
#13993=CARTESIAN_POINT('Ctrl Pts',(10.5341220579192,1.21401666636749,-0.000470252816738081));
#13994=CARTESIAN_POINT('Ctrl Pts',(10.5235196325477,1.20343268662274,0.201991562854702));
#13995=CARTESIAN_POINT('Ctrl Pts',(10.5129172908767,1.19284910679518,0.404453403808947));
#13996=CARTESIAN_POINT('Ctrl Pts',(10.5023149573519,1.18226542681329,0.606915239027137));
#13997=CARTESIAN_POINT('Ctrl Pts',(10.5827170203615,1.18801090922716,0.000717463067903341));
#13998=CARTESIAN_POINT('Ctrl Pts',(10.5721088691741,1.17742555398174,0.203178921531494));
#13999=CARTESIAN_POINT('Ctrl Pts',(10.5615007184277,1.16684027916303,0.405640383775807));
#14000=CARTESIAN_POINT('Ctrl Pts',(10.5508925935528,1.15625520969485,0.60810185787831));
#14001=CARTESIAN_POINT('Ctrl Pts',(10.5997792798033,1.13754603572512,-0.00102559206997387));
#14002=CARTESIAN_POINT('Ctrl Pts',(10.5891686973038,1.12696411138589,0.201435946515793));
#14003=CARTESIAN_POINT('Ctrl Pts',(10.5785581831385,1.11638231376635,0.40389749513889));
#14004=CARTESIAN_POINT('Ctrl Pts',(10.5679475995174,1.10580071474959,0.606359050464716));
#14005=CARTESIAN_POINT('Ctrl Pts',(10.5998382764002,1.11594571320176,-0.00215131420076595));
#14006=CARTESIAN_POINT('Ctrl Pts',(10.5892277121014,1.10536524516024,0.200310313518148));
#14007=CARTESIAN_POINT('Ctrl Pts',(10.5786171473394,1.09478494672192,0.402771950076102));
#14008=CARTESIAN_POINT('Ctrl Pts',(10.5680065821063,1.08420482079361,0.605233595624295));
#14009=CARTESIAN_POINT('Ctrl Pts',(10.5680065821063,1.08420482079361,0.605233595624295));
#14010=CARTESIAN_POINT('Ctrl Pts',(10.5785795654695,1.09474747266587,0.40348905487273));
#14011=CARTESIAN_POINT('Ctrl Pts',(10.589152548365,1.10529029582828,0.201744523047831));
#14012=CARTESIAN_POINT('Ctrl Pts',(10.5997255308004,1.11583328740478,1.07661275727811E-16));
#14013=CARTESIAN_POINT('Ctrl Pts',(10.1947388861048,1.09885088260187,0.7));
#14014=CARTESIAN_POINT('Ctrl Pts',(10.285877616441,1.09404209584202,0.7));
#14015=CARTESIAN_POINT('Ctrl Pts',(10.3770124662346,1.0891584122264,0.7));
#14016=CARTESIAN_POINT('Ctrl Pts',(10.4681436286308,1.08420482079361,0.7));
#14017=CARTESIAN_POINT('Ctrl Pts',(10.196260416419,1.12768774893097,0.700000000000001));
#14018=CARTESIAN_POINT('Ctrl Pts',(10.2874149314686,1.12287675076168,0.699999949550842));
#14019=CARTESIAN_POINT('Ctrl Pts',(10.3785648662465,1.11799094453753,0.700000051218742));
#14020=CARTESIAN_POINT('Ctrl Pts',(10.4697107510168,1.11303515260326,0.7));
#14021=CARTESIAN_POINT('Ctrl Pts',(10.1988975981852,1.17766904563614,0.67669140632491));
#14022=CARTESIAN_POINT('Ctrl Pts',(10.2900793016129,1.17285439035486,0.676693724638983));
#14023=CARTESIAN_POINT('Ctrl Pts',(10.3812557252598,1.16796482352885,0.676696026813929));
#14024=CARTESIAN_POINT('Ctrl Pts',(10.4724269697127,1.16300539549315,0.676698381019544));
#14025=CARTESIAN_POINT('Ctrl Pts',(10.1999375452555,1.19737868557977,0.627098033786781));
#14026=CARTESIAN_POINT('Ctrl Pts',(10.2911301919381,1.19256517083271,0.627104033151799));
#14027=CARTESIAN_POINT('Ctrl Pts',(10.382317043787,1.18767684023183,0.627110048826767));
#14028=CARTESIAN_POINT('Ctrl Pts',(10.4734985149421,1.18271860027509,0.627116141711795));
#14029=CARTESIAN_POINT('Ctrl Pts',(10.1999999975038,1.19856231440453,0.605472757505366));
#14030=CARTESIAN_POINT('Ctrl Pts',(10.2911933328565,1.19375025772558,0.605479840815741));
#14031=CARTESIAN_POINT('Ctrl Pts',(10.3823809652617,1.18886335120032,0.605486986548286));
#14032=CARTESIAN_POINT('Ctrl Pts',(10.4735630903435,1.18390659316268,0.605494180667944));
#14033=CARTESIAN_POINT('Ctrl Pts',(0.200159601751749,1.12312829248604,-0.00219180147311912));
#14034=CARTESIAN_POINT('Ctrl Pts',(0.210770873167554,1.11255922017607,0.200283318842441));
#14035=CARTESIAN_POINT('Ctrl Pts',(0.221382145211419,1.10199037808008,0.402758451142111));
#14036=CARTESIAN_POINT('Ctrl Pts',(0.231993417893744,1.09142177001972,0.605233595624295));
#14037=CARTESIAN_POINT('Ctrl Pts',(0.200236952094631,1.15148086499205,-0.000715869007730825));
#14038=CARTESIAN_POINT('Ctrl Pts',(0.210848310847714,1.14090905181173,0.201759082033021));
#14039=CARTESIAN_POINT('Ctrl Pts',(0.221459381762758,1.13033759660317,0.404234066901971));
#14040=CARTESIAN_POINT('Ctrl Pts',(0.232070742664217,1.11976621744484,0.606709040139042));
#14041=CARTESIAN_POINT('Ctrl Pts',(0.222806696702742,1.20067708175657,0.000669311976984441));
#14042=CARTESIAN_POINT('Ctrl Pts',(0.233413416075889,1.19010082554658,0.203144236955742));
#14043=CARTESIAN_POINT('Ctrl Pts',(0.244020198555212,1.17952469009474,0.405619164345205));
#14044=CARTESIAN_POINT('Ctrl Pts',(0.254626870458834,1.16894881850735,0.608094110943904));
#14045=CARTESIAN_POINT('Ctrl Pts',(0.271086891015657,1.22096622390789,-0.000801865493577694));
#14046=CARTESIAN_POINT('Ctrl Pts',(0.281686280594249,1.21039315447922,0.201673594461172));
#14047=CARTESIAN_POINT('Ctrl Pts',(0.292285672737775,1.1998203699977,0.404149068703718));
#14048=CARTESIAN_POINT('Ctrl Pts',(0.302884933932915,1.18924771644243,0.606624555877912));
#14049=CARTESIAN_POINT('Ctrl Pts',(0.292287201081515,1.22267118699778,-0.00182392867695869));
#14050=CARTESIAN_POINT('Ctrl Pts',(0.302884364349574,1.21210098433295,0.200651796350731));
#14051=CARTESIAN_POINT('Ctrl Pts',(0.313481451159089,1.20153100270242,0.403127536304793));
#14052=CARTESIAN_POINT('Ctrl Pts',(0.324078460244491,1.19096124572524,0.605603291426262));
#14053=CARTESIAN_POINT('Origin',(10.6002740930491,1.4,-0.0104671912485891));
#14054=CARTESIAN_POINT('Origin',(0.331856371369202,1.09142177001972,0.6));
#14055=CARTESIAN_POINT('',(0.3318563713692,1.09142177001972,0.9));
#14056=CARTESIAN_POINT('',(0.0322675109428288,1.09142177001972,0.615700786872883));
#14057=CARTESIAN_POINT('Origin',(0.3318563713692,1.09142177001972,0.6));
#14058=CARTESIAN_POINT('',(0.308522637995069,1.39004019713626,0.616809874278785));
#14059=CARTESIAN_POINT('Origin',(0.331856371369202,1.09142177001972,0.6));
#14060=CARTESIAN_POINT('Origin',(0.331856371369201,1.09142177001972,0.6));
#14061=CARTESIAN_POINT('Origin',(10.4681436286308,1.08420482079361,0.6));
#14062=CARTESIAN_POINT('',(10.4681436286308,1.08420482109828,0.9));
#14063=CARTESIAN_POINT('',(10.4844020137689,1.3833101379008,0.616482542003833));
#14064=CARTESIAN_POINT('Origin',(10.4681436258201,1.08420482094639,0.6));
#14065=CARTESIAN_POINT('',(10.7677324890572,1.08420482079361,0.615700786872884));
#14066=CARTESIAN_POINT('Origin',(10.4681436286308,1.08420482079361,0.6));
#14067=CARTESIAN_POINT('Origin',(10.4681436286308,1.08420482079362,0.6));
#14068=CARTESIAN_POINT('Origin',(0.3318563713692,-1.09142177001972,0.6));
#14069=CARTESIAN_POINT('',(0.3318563713692,-1.09142177001972,0.9));
#14070=CARTESIAN_POINT('',(0.308522637995069,-1.39004019713626,0.616809874278785));
#14071=CARTESIAN_POINT('Origin',(0.3318563713692,-1.09142177001972,0.6));
#14072=CARTESIAN_POINT('',(0.0322675109428289,-1.09142177001972,0.615700786872884));
#14073=CARTESIAN_POINT('Origin',(0.3318563713692,-1.09142177001972,0.6));
#14074=CARTESIAN_POINT('Origin',(0.331856371369201,-1.09142177001972,0.6));
#14075=CARTESIAN_POINT('Origin',(0.3318563713692,-0.7,0.6));
#14076=CARTESIAN_POINT('',(0.0322675109428288,-0.7,0.615700786872883));
#14077=CARTESIAN_POINT('',(0.3318563713692,-0.7,0.9));
#14078=CARTESIAN_POINT('Ctrl Pts',(0.276048389810261,-1.42252533450788,
-0.00533608639730399));
#14079=CARTESIAN_POINT('Ctrl Pts',(0.28687338241706,-1.4116967417008,0.202045878554724));
#14080=CARTESIAN_POINT('Ctrl Pts',(0.297698133178874,-1.40086836142621,
0.409427865329919));
#14081=CARTESIAN_POINT('Ctrl Pts',(0.308522637995069,-1.39004019713626,
0.616809874278785));
#14082=CARTESIAN_POINT('Ctrl Pts',(0.191246496057484,-1.41570630783033,
-0.00124775669238285));
#14083=CARTESIAN_POINT('Ctrl Pts',(0.202080757839133,-1.40486573978029,
0.206133102090467));
#14084=CARTESIAN_POINT('Ctrl Pts',(0.212914648880055,-1.39402634701096,
0.413514041581016));
#14085=CARTESIAN_POINT('Ctrl Pts',(0.223748532748767,-1.38318608000504,
0.620894932085382));
#14086=CARTESIAN_POINT('Ctrl Pts',(0.0492682973509243,-1.33685850703924,
0.00207719607616587));
#14087=CARTESIAN_POINT('Ctrl Pts',(0.0601266125734448,-1.32601270457081,
0.209456583216085));
#14088=CARTESIAN_POINT('Ctrl Pts',(0.0709850253737815,-1.3151666447344,
0.416835949794532));
#14089=CARTESIAN_POINT('Ctrl Pts',(0.0818432319483421,-1.30432109509162,
0.624215353109623));
#14090=CARTESIAN_POINT('Ctrl Pts',(-0.000163444061205068,-1.18769013309795,
-0.00311869847265479));
#14091=CARTESIAN_POINT('Ctrl Pts',(0.0107049555364969,-1.17685886333949,
0.204261034729081));
#14092=CARTESIAN_POINT('Ctrl Pts',(0.0215730900970294,-1.16602762920277,
0.411640782964944));
#14093=CARTESIAN_POINT('Ctrl Pts',(0.0324414916763936,-1.15519677672624,
0.619020537031064));
#14094=CARTESIAN_POINT('Ctrl Pts',(-0.00033748371827097,-1.12389640457412,
-0.0064395729582146));
#14095=CARTESIAN_POINT('Ctrl Pts',(0.0105308471731094,-1.11307128361434,
0.200940534347673));
#14096=CARTESIAN_POINT('Ctrl Pts',(0.0213991787230862,-1.10224640406117,
0.408320654220332));
#14097=CARTESIAN_POINT('Ctrl Pts',(0.0322675109428289,-1.09142177001972,
0.615700786872884));
#14098=CARTESIAN_POINT('Ctrl Pts',(0.27632692456468,-1.42224670711126,5.13911829758129E-17));
#14099=CARTESIAN_POINT('Ctrl Pts',(0.287059068122268,-1.41151099373342,
0.20560326985903));
#14100=CARTESIAN_POINT('Ctrl Pts',(0.297790973931072,-1.40077548928706,
0.411206561171438));
#14101=CARTESIAN_POINT('Ctrl Pts',(0.308522637995069,-1.39004019713626,
0.616809874278785));
#14102=CARTESIAN_POINT('Ctrl Pts',(0.0322675109428289,-1.09142177001972,
0.615700786872884));
#14103=CARTESIAN_POINT('Ctrl Pts',(0.0215116733095221,-1.10213436178043,
0.410467178800746));
#14104=CARTESIAN_POINT('Ctrl Pts',(0.0107558363321879,-1.11284719399673,
0.205233583245308));
#14105=CARTESIAN_POINT('Ctrl Pts',(1.76901136968166E-16,-1.12356026268968,
-7.45931094670027E-17));
#14106=CARTESIAN_POINT('Origin',(10.4681436286308,-1.08420482109828,0.6));
#14107=CARTESIAN_POINT('',(10.7677324890572,-1.08420482079361,0.615700786872884));
#14108=CARTESIAN_POINT('',(10.4844020137689,-1.3833101379008,0.616482542003833));
#14109=CARTESIAN_POINT('Origin',(10.4681436286308,-1.08420482079361,0.600000000000001));
#14110=CARTESIAN_POINT('',(10.4681436258201,-1.08420482094639,0.9));
#14111=CARTESIAN_POINT('Origin',(10.4681436286308,-1.08420482109828,0.6));
#14112=CARTESIAN_POINT('Origin',(10.4681436286308,-1.08420482079361,0.6));
#14113=CARTESIAN_POINT('Origin',(10.4681436286308,0.7,0.6));
#14114=CARTESIAN_POINT('',(10.7677324890572,0.7,0.615700786872884));
#14115=CARTESIAN_POINT('',(10.4681436286308,0.7,0.9));
#14116=CARTESIAN_POINT('Ctrl Pts',(10.4681436286308,-1.08420482079361,0.9));
#14117=CARTESIAN_POINT('Ctrl Pts',(9.02115959826777,-1.16285813221549,0.9));
#14118=CARTESIAN_POINT('Ctrl Pts',(5.64262097844114,-1.30550334054488,0.9));
#14119=CARTESIAN_POINT('Ctrl Pts',(2.25816172369615,-1.24194126716656,0.9));
#14120=CARTESIAN_POINT('Ctrl Pts',(0.331856371369198,-1.09142177001972,
0.9));
#14121=CARTESIAN_POINT('Ctrl Pts',(10.4728449957889,-1.17069581622255,0.9));
#14122=CARTESIAN_POINT('Ctrl Pts',(9.02515960257209,-1.24945398332951,0.900002463983243));
#14123=CARTESIAN_POINT('Ctrl Pts',(5.64406008560805,-1.39235654229312,0.899995181674544));
#14124=CARTESIAN_POINT('Ctrl Pts',(2.25481214769604,-1.3286896492945,0.900006992415263));
#14125=CARTESIAN_POINT('Ctrl Pts',(0.325113511056834,-1.17771496230318,
0.9));
#14126=CARTESIAN_POINT('Ctrl Pts',(10.4809942371438,-1.32061731204901,0.830050158657121));
#14127=CARTESIAN_POINT('Ctrl Pts',(9.03210079995546,-1.3995487214628,0.829938185878055));
#14128=CARTESIAN_POINT('Ctrl Pts',(5.64656962219688,-1.54290142969263,0.82970437227026));
#14129=CARTESIAN_POINT('Ctrl Pts',(2.24896854757963,-1.47903552984056,0.829838703712927));
#14130=CARTESIAN_POINT('Ctrl Pts',(0.313425270489114,-1.32729771265557,
0.830156825336737));
#14131=CARTESIAN_POINT('Ctrl Pts',(10.4842082875648,-1.37974615923803,0.681348425135383));
#14132=CARTESIAN_POINT('Ctrl Pts',(9.03482793853036,-1.45862084618981,0.681058092399338));
#14133=CARTESIAN_POINT('Ctrl Pts',(5.64753778607331,-1.60187726023264,0.68045297450285));
#14134=CARTESIAN_POINT('Ctrl Pts',(2.24670449952385,-1.53809938127555,0.680799765935021));
#14135=CARTESIAN_POINT('Ctrl Pts',(0.308806004580392,-1.38641375285276,
0.681625057916928));
#14136=CARTESIAN_POINT('Ctrl Pts',(10.4844020137689,-1.3833101379008,0.616482542003833));
#14137=CARTESIAN_POINT('Ctrl Pts',(9.03499042108131,-1.46211428773623,0.616139856494792));
#14138=CARTESIAN_POINT('Ctrl Pts',(5.64759185703765,-1.60522711936681,0.615422163720642));
#14139=CARTESIAN_POINT('Ctrl Pts',(2.24657199659733,-1.54153220865049,0.615835494619844));
#14140=CARTESIAN_POINT('Ctrl Pts',(0.308522637995066,-1.39004019713626,
0.616809874278785));
#14141=CARTESIAN_POINT('Ctrl Pts',(0.308522637995066,-1.39004019713626,
0.616809874278785));
#14142=CARTESIAN_POINT('Ctrl Pts',(2.24657199659733,-1.54153220865049,0.615835494619844));
#14143=CARTESIAN_POINT('Ctrl Pts',(5.64759185703765,-1.60522711936681,0.615422163720642));
#14144=CARTESIAN_POINT('Ctrl Pts',(9.03499042108131,-1.46211428773623,0.616139856494792));
#14145=CARTESIAN_POINT('Ctrl Pts',(10.4844020137689,-1.3833101379008,0.616482542003833));
#14146=CARTESIAN_POINT('Ctrl Pts',(10.4681436258201,-1.08420482094639,0.900000000000001));
#14147=CARTESIAN_POINT('Ctrl Pts',(9.02115959639274,-1.16285813229465,0.9));
#14148=CARTESIAN_POINT('Ctrl Pts',(5.64262097750198,-1.30550334052724,0.9));
#14149=CARTESIAN_POINT('Ctrl Pts',(2.25816172369615,-1.24194126716656,0.9));
#14150=CARTESIAN_POINT('Ctrl Pts',(0.331856371369198,-1.09142177001972,
0.9));
#14151=CARTESIAN_POINT('Ctrl Pts',(10.8003433549902,-1.11672267507076,-0.00655160349952438));
#14152=CARTESIAN_POINT('Ctrl Pts',(10.7894730668347,-1.10588321133639,0.200865850630566));
#14153=CARTESIAN_POINT('Ctrl Pts',(10.7786027781932,-1.09504392553578,0.408283314033857));
#14154=CARTESIAN_POINT('Ctrl Pts',(10.7677324890572,-1.08420482079361,0.615700786872885));
#14155=CARTESIAN_POINT('Ctrl Pts',(10.8001073672393,-1.20312439623403,-0.00204868896805508));
#14156=CARTESIAN_POINT('Ctrl Pts',(10.7892368724076,-1.19227880391739,0.205368384315645));
#14157=CARTESIAN_POINT('Ctrl Pts',(10.7783670568079,-1.18143370221047,0.41278551899075));
#14158=CARTESIAN_POINT('Ctrl Pts',(10.7674965587017,-1.17058839661753,0.620202606234566));
#14159=CARTESIAN_POINT('Ctrl Pts',(10.7300137544668,-1.35289768637741,0.00210488808650419));
#14160=CARTESIAN_POINT('Ctrl Pts',(10.7191538066016,-1.34204221082848,0.209521911971666));
#14161=CARTESIAN_POINT('Ctrl Pts',(10.7082938463195,-1.33118673671862,0.416938933985702));
#14162=CARTESIAN_POINT('Ctrl Pts',(10.6974340169938,-1.32033143065575,0.624355970618915));
#14163=CARTESIAN_POINT('Ctrl Pts',(10.5816241002662,-1.4121605627967,-0.00257485550010117));
#14164=CARTESIAN_POINT('Ctrl Pts',(10.5707805459565,-1.4013126969686,0.204843391064434));
#14165=CARTESIAN_POINT('Ctrl Pts',(10.5599369567012,-1.39046512672587,0.412261650129749));
#14166=CARTESIAN_POINT('Ctrl Pts',(10.5490937145378,-1.37961751361469,0.619679923312015));
#14167=CARTESIAN_POINT('Ctrl Pts',(10.5169176890673,-1.41583338198674,-0.00577403633861717));
#14168=CARTESIAN_POINT('Ctrl Pts',(10.5060789456421,-1.40499213715574,0.201644806368331));
#14169=CARTESIAN_POINT('Ctrl Pts',(10.4952403861233,-1.39415105487295,0.40906366572247));
#14170=CARTESIAN_POINT('Ctrl Pts',(10.4844020137689,-1.3833101379008,0.616482542003833));
#14171=CARTESIAN_POINT('Ctrl Pts',(10.8,-1.11638029377732,-2.51534904016637E-17));
#14172=CARTESIAN_POINT('Ctrl Pts',(10.7892441634977,-1.10565496086826,0.205233586491178));
#14173=CARTESIAN_POINT('Ctrl Pts',(10.7784883265195,-1.09492980219801,0.410467182062988));
#14174=CARTESIAN_POINT('Ctrl Pts',(10.7677324890572,-1.08420482079361,0.615700786872885));
#14175=CARTESIAN_POINT('Ctrl Pts',(10.4844020137689,-1.3833101379008,0.616482542003833));
#14176=CARTESIAN_POINT('Ctrl Pts',(10.4951398148107,-1.39405045994841,0.410988344812119));
#14177=CARTESIAN_POINT('Ctrl Pts',(10.5058777995597,-1.40479094425298,0.205494164234945));
#14178=CARTESIAN_POINT('Ctrl Pts',(10.5166159648474,-1.4155315881283,-2.5652223401007E-16));
#14179=CARTESIAN_POINT('Ctrl Pts',(10.5169125872774,1.41582827901939,-0.0056764044152427));
#14180=CARTESIAN_POINT('Ctrl Pts',(10.5060755445066,1.40498873522851,0.20170989432247));
#14181=CARTESIAN_POINT('Ctrl Pts',(10.4952386855848,1.39414935393528,0.409096209702196));
#14182=CARTESIAN_POINT('Ctrl Pts',(10.4844020137689,1.3833101379008,0.616482542003833));
#14183=CARTESIAN_POINT('Ctrl Pts',(10.6031877991504,1.41093118264609,-0.00141083033817288));
#14184=CARTESIAN_POINT('Ctrl Pts',(10.5923442181457,1.40008262840665,0.205974657203891));
#14185=CARTESIAN_POINT('Ctrl Pts',(10.5815009048179,1.38923496752292,0.413360205434192));
#14186=CARTESIAN_POINT('Ctrl Pts',(10.5706576147941,1.37838663885266,0.62074571708141));
#14187=CARTESIAN_POINT('Ctrl Pts',(10.7489822201969,1.33286898269122,0.00215046584238339));
#14188=CARTESIAN_POINT('Ctrl Pts',(10.7381210493968,1.32201618867047,0.209534855263179));
#14189=CARTESIAN_POINT('Ctrl Pts',(10.7272598662103,1.31116338896628,0.416919242515175));
#14190=CARTESIAN_POINT('Ctrl Pts',(10.716398780155,1.30031077634578,0.624303643734563));
#14191=CARTESIAN_POINT('Ctrl Pts',(10.8001612475457,1.18151886169146,-0.00307678645922502));
#14192=CARTESIAN_POINT('Ctrl Pts',(10.7892926103682,1.17067663552019,0.20430785074418));
#14193=CARTESIAN_POINT('Ctrl Pts',(10.7784241800195,1.15983442267521,0.41169249890798));
#14194=CARTESIAN_POINT('Ctrl Pts',(10.7675555412906,1.14899250266155,0.619077151394146));
#14195=CARTESIAN_POINT('Ctrl Pts',(10.8003382383521,1.11671757294177,-0.00645397222975308));
#14196=CARTESIAN_POINT('Ctrl Pts',(10.7894696557425,1.1058798099729,0.200930938146656));
#14197=CARTESIAN_POINT('Ctrl Pts',(10.778601072647,1.09504222488243,0.408315857793383));
#14198=CARTESIAN_POINT('Ctrl Pts',(10.7677324890572,1.08420482079361,0.615700786872884));
#14199=CARTESIAN_POINT('Ctrl Pts',(10.5166159648474,1.4155315881283,3.37837396946483E-16));
#14200=CARTESIAN_POINT('Ctrl Pts',(10.5058777995597,1.40479094425298,0.205494164234944));
#14201=CARTESIAN_POINT('Ctrl Pts',(10.4951398148107,1.39405045994841,0.41098834481212));
#14202=CARTESIAN_POINT('Ctrl Pts',(10.4844020137689,1.3833101379008,0.616482542003833));
#14203=CARTESIAN_POINT('Ctrl Pts',(10.7677324890572,1.08420482079361,0.615700786872884));
#14204=CARTESIAN_POINT('Ctrl Pts',(10.7784883265195,1.09492980219801,0.410467182062988));
#14205=CARTESIAN_POINT('Ctrl Pts',(10.7892441634977,1.10565496086826,0.205233586491177));
#14206=CARTESIAN_POINT('Ctrl Pts',(10.8,1.11638029377732,-4.7271214720368E-17));
#14207=CARTESIAN_POINT('Ctrl Pts',(0.3318563713692,1.09142177001972,0.9));
#14208=CARTESIAN_POINT('Ctrl Pts',(1.77658538561441,1.20431139287985,0.9));
#14209=CARTESIAN_POINT('Ctrl Pts',(5.15852145577913,1.31798734362749,0.900000000000001));
#14210=CARTESIAN_POINT('Ctrl Pts',(8.53883158814675,1.18907590268945,0.9));
#14211=CARTESIAN_POINT('Ctrl Pts',(10.4681436286308,1.08420482079361,0.9));
#14212=CARTESIAN_POINT('Ctrl Pts',(0.325113511056836,1.17771496230318,0.9));
#14213=CARTESIAN_POINT('Ctrl Pts',(1.77238748853623,1.29094597754667,0.900005244311447));
#14214=CARTESIAN_POINT('Ctrl Pts',(5.15940689953628,1.40489117512763,0.899995532233175));
#14215=CARTESIAN_POINT('Ctrl Pts',(8.54259780483314,1.2757067056985,0.90000328531099));
#14216=CARTESIAN_POINT('Ctrl Pts',(10.4728449957889,1.17069581622255,0.9));
#14217=CARTESIAN_POINT('Ctrl Pts',(0.313425270489116,1.32729771265557,0.830156825336737));
#14218=CARTESIAN_POINT('Ctrl Pts',(1.76508272830699,1.44110107554431,0.829918234118879));
#14219=CARTESIAN_POINT('Ctrl Pts',(5.16095094050242,1.55552201031752,0.829677185710002));
#14220=CARTESIAN_POINT('Ctrl Pts',(8.54913632089268,1.4258591912674,0.829900861618366));
#14221=CARTESIAN_POINT('Ctrl Pts',(10.4809942371438,1.32061731204901,0.830050158657121));
#14222=CARTESIAN_POINT('Ctrl Pts',(0.308806004580394,1.38641375285276,0.681625057916928));
#14223=CARTESIAN_POINT('Ctrl Pts',(1.76222987578798,1.50017797416985,0.681006088930498));
#14224=CARTESIAN_POINT('Ctrl Pts',(5.16154986224672,1.61450132085358,0.68038246417749));
#14225=CARTESIAN_POINT('Ctrl Pts',(8.55170115551887,1.48491240850707,0.680961314820656));
#14226=CARTESIAN_POINT('Ctrl Pts',(10.4842082875648,1.37974615923803,0.681348425135383));
#14227=CARTESIAN_POINT('Ctrl Pts',(0.308522637995068,1.39004019713626,0.616809874278785));
#14228=CARTESIAN_POINT('Ctrl Pts',(1.76205965694675,1.50365920577193,0.616079089534579));
#14229=CARTESIAN_POINT('Ctrl Pts',(5.16158497046229,1.61783515152865,0.615338844765104));
#14230=CARTESIAN_POINT('Ctrl Pts',(8.55185322351876,1.48838233768137,0.616025627991778));
#14231=CARTESIAN_POINT('Ctrl Pts',(10.4844020137689,1.3833101379008,0.616482542003833));
#14232=CARTESIAN_POINT('Ctrl Pts',(10.4844020137689,1.3833101379008,0.616482542003833));
#14233=CARTESIAN_POINT('Ctrl Pts',(8.55185322351876,1.48838233768137,0.616025627991778));
#14234=CARTESIAN_POINT('Ctrl Pts',(5.16158497046229,1.61783515152865,0.615338844765104));
#14235=CARTESIAN_POINT('Ctrl Pts',(1.76205965694675,1.50365920577193,0.616079089534579));
#14236=CARTESIAN_POINT('Ctrl Pts',(0.308522637995068,1.39004019713626,0.616809874278785));
#14237=CARTESIAN_POINT('Ctrl Pts',(0.3318563713692,1.09142177001972,0.9));
#14238=CARTESIAN_POINT('Ctrl Pts',(1.77658538561441,1.20431139287985,0.9));
#14239=CARTESIAN_POINT('Ctrl Pts',(5.15852145577913,1.31798734362749,0.900000000000001));
#14240=CARTESIAN_POINT('Ctrl Pts',(8.53883158814675,1.18907590268945,0.9));
#14241=CARTESIAN_POINT('Ctrl Pts',(10.4681436286308,1.08420482079361,0.9));
#14242=CARTESIAN_POINT('Ctrl Pts',(-0.000344602063817145,1.12390349461883,
-0.00657539908256866));
#14243=CARTESIAN_POINT('Ctrl Pts',(0.0105261016091243,1.11307601020539,
0.200849983592616));
#14244=CARTESIAN_POINT('Ctrl Pts',(0.0213968059409475,1.10224876730309,
0.408275378840013));
#14245=CARTESIAN_POINT('Ctrl Pts',(0.0322675109428289,1.09142177001972,
0.615700786872884));
#14246=CARTESIAN_POINT('Ctrl Pts',(-0.000112549170678945,1.2089618047365,
-0.00214756610981592));
#14247=CARTESIAN_POINT('Ctrl Pts',(0.0107584275574203,1.19812589474889,
0.205277296000037));
#14248=CARTESIAN_POINT('Ctrl Pts',(0.021628504370896,1.18729063034778,0.412702239156743));
#14249=CARTESIAN_POINT('Ctrl Pts',(0.0324994852542487,1.17645511229507,
0.620127120417125));
#14250=CARTESIAN_POINT('Ctrl Pts',(0.0675181008536004,1.35659180908255,
0.00201426213057289));
#14251=CARTESIAN_POINT('Ctrl Pts',(0.0783748317004002,1.34574224493831,
0.20943904356877));
#14252=CARTESIAN_POINT('Ctrl Pts',(0.0892318011706237,1.33489254525337,
0.416863803530356));
#14253=CARTESIAN_POINT('Ctrl Pts',(0.100088380073201,1.32404321751407,0.624288602298589));
#14254=CARTESIAN_POINT('Ctrl Pts',(0.212439875011655,1.41741816253371,-0.00240566592686199));
#14255=CARTESIAN_POINT('Ctrl Pts',(0.223274062163905,1.40657840226088,0.20502076110302));
#14256=CARTESIAN_POINT('Ctrl Pts',(0.234108278795672,1.39573903465802,0.412447205628077));
#14257=CARTESIAN_POINT('Ctrl Pts',(0.244942059060342,1.38489960928785,0.619873667633733));
#14258=CARTESIAN_POINT('Ctrl Pts',(0.276041299849618,1.42253242682652,-0.00547191373834488));
#14259=CARTESIAN_POINT('Ctrl Pts',(0.286868655882245,1.41170146982041,0.201955326984501));
#14260=CARTESIAN_POINT('Ctrl Pts',(0.297695769965166,1.40087072543886,0.409382589539965));
#14261=CARTESIAN_POINT('Ctrl Pts',(0.308522637995069,1.39004019713626,0.616809874278785));
#14262=CARTESIAN_POINT('Ctrl Pts',(2.26869304592592E-17,1.12356026268968,
-3.16587034365767E-17));
#14263=CARTESIAN_POINT('Ctrl Pts',(0.0107558363321878,1.11284719399672,
0.205233583245308));
#14264=CARTESIAN_POINT('Ctrl Pts',(0.0215116733095221,1.10213436178043,
0.410467178800746));
#14265=CARTESIAN_POINT('Ctrl Pts',(0.0322675109428289,1.09142177001972,
0.615700786872884));
#14266=CARTESIAN_POINT('Ctrl Pts',(0.308522637995069,1.39004019713626,0.616809874278785));
#14267=CARTESIAN_POINT('Ctrl Pts',(0.297790973931072,1.40077548928706,0.411206561171438));
#14268=CARTESIAN_POINT('Ctrl Pts',(0.287059068122271,1.41151099373341,0.205603269859031));
#14269=CARTESIAN_POINT('Ctrl Pts',(0.276326924564681,1.42224670711126,-2.68882138776405E-16));
#14270=CARTESIAN_POINT('Ctrl Pts',(10.5166159648474,-1.4155315881283,0.));
#14271=CARTESIAN_POINT('Ctrl Pts',(10.5064062201588,-1.40475637621136,0.205603291426271));
#14272=CARTESIAN_POINT('Ctrl Pts',(10.4961964754701,-1.39398116429443,0.411206582852543));
#14273=CARTESIAN_POINT('Ctrl Pts',(10.4859867307814,-1.38320595237749,0.616809874278814));
#14274=CARTESIAN_POINT('Ctrl Pts',(7.10318628475318,-1.599994843061,0.));
#14275=CARTESIAN_POINT('Ctrl Pts',(7.09978773046573,-1.58921963114407,0.205603291426271));
#14276=CARTESIAN_POINT('Ctrl Pts',(7.09638917617828,-1.57844441922713,0.411206582852543));
#14277=CARTESIAN_POINT('Ctrl Pts',(7.09299062189083,-1.5676692073102,0.616809874278814));
#14278=CARTESIAN_POINT('Ctrl Pts',(3.68975660465893,-1.68747752195839,0.));
#14279=CARTESIAN_POINT('Ctrl Pts',(3.69316924077269,-1.67670231004145,0.205603291426272));
#14280=CARTESIAN_POINT('Ctrl Pts',(3.69658187688646,-1.66592709812452,0.411206582852543));
#14281=CARTESIAN_POINT('Ctrl Pts',(3.69999451300023,-1.65515188620758,0.616809874278814));
#14282=CARTESIAN_POINT('Ctrl Pts',(0.276326924564679,-1.42224670711126,
0.));
#14283=CARTESIAN_POINT('Ctrl Pts',(0.286550751079662,-1.41147149519433,
0.205603291426271));
#14284=CARTESIAN_POINT('Ctrl Pts',(0.296774577594646,-1.40069628327739,
0.411206582852543));
#14285=CARTESIAN_POINT('Ctrl Pts',(0.306998404109629,-1.38992107136046,
0.616809874278814));
#14286=CARTESIAN_POINT('Origin',(0.,-1.4,0.));
#14287=CARTESIAN_POINT('Origin',(5.4,-8.13935059369636E-18,0.9));
#14288=CARTESIAN_POINT('Ctrl Pts',(0.276326924564679,1.42224670711126,0.));
#14289=CARTESIAN_POINT('Ctrl Pts',(0.286550751079662,1.41147149519433,0.205603291426271));
#14290=CARTESIAN_POINT('Ctrl Pts',(0.296774577594645,1.40069628327739,0.411206582852543));
#14291=CARTESIAN_POINT('Ctrl Pts',(0.306998404109628,1.38992107136046,0.616809874278814));
#14292=CARTESIAN_POINT('Ctrl Pts',(3.68975660465893,1.68747752195839,0.));
#14293=CARTESIAN_POINT('Ctrl Pts',(3.6931692407727,1.67670231004145,0.205603291426271));
#14294=CARTESIAN_POINT('Ctrl Pts',(3.69658187688646,1.66592709812452,0.411206582852543));
#14295=CARTESIAN_POINT('Ctrl Pts',(3.69999451300023,1.65515188620758,0.616809874278814));
#14296=CARTESIAN_POINT('Ctrl Pts',(7.10318628475318,1.599994843061,0.));
#14297=CARTESIAN_POINT('Ctrl Pts',(7.09978773046573,1.58921963114407,0.205603291426271));
#14298=CARTESIAN_POINT('Ctrl Pts',(7.09638917617828,1.57844441922713,0.411206582852543));
#14299=CARTESIAN_POINT('Ctrl Pts',(7.09299062189083,1.5676692073102,0.616809874278814));
#14300=CARTESIAN_POINT('Ctrl Pts',(10.5166159648474,1.4155315881283,0.));
#14301=CARTESIAN_POINT('Ctrl Pts',(10.5064062201588,1.40475637621136,0.205603291426271));
#14302=CARTESIAN_POINT('Ctrl Pts',(10.4961964754701,1.39398116429443,0.411206582852543));
#14303=CARTESIAN_POINT('Ctrl Pts',(10.4859867307814,1.38320595237749,0.616809874278814));
#14304=CARTESIAN_POINT('Origin',(10.8,1.4,0.));
#14305=CARTESIAN_POINT('',(0.,0.,0.));
#14306=CARTESIAN_POINT('Origin',(8.1,-1.,0.7));
#14307=CARTESIAN_POINT('',(7.94916965151797,-1.19937453693185,0.7));
#14308=CARTESIAN_POINT('',(8.26514540988519,-1.18768855477586,0.7));
#14309=CARTESIAN_POINT('Ctrl Pts',(7.94916965151797,-1.19937453693185,0.7));
#14310=CARTESIAN_POINT('Ctrl Pts',(7.97160858810976,-1.21634998764782,0.7));
#14311=CARTESIAN_POINT('Ctrl Pts',(7.99739856866269,-1.22989011121344,0.69528529300377));
#14312=CARTESIAN_POINT('Ctrl Pts',(8.03944443766207,-1.24298414277179,0.688517705185315));
#14313=CARTESIAN_POINT('Ctrl Pts',(8.05362924383607,-1.24609346022897,0.686388676887586));
#14314=CARTESIAN_POINT('Ctrl Pts',(8.075506183533,-1.24890990228851,0.684139035126277));
#14315=CARTESIAN_POINT('Ctrl Pts',(8.08297567221474,-1.24953307703463,0.683546226354886));
#14316=CARTESIAN_POINT('Ctrl Pts',(8.0940066533036,-1.24995288972095,0.68299521602547));
#14317=CARTESIAN_POINT('Ctrl Pts',(8.09752287926269,-1.25001251279495,0.68286729538075));
#14318=CARTESIAN_POINT('Ctrl Pts',(8.10293413375911,-1.249989933108,0.682747340264197));
#14319=CARTESIAN_POINT('Ctrl Pts',(8.10482478940148,-1.24996059450444,0.682719828470948));
#14320=CARTESIAN_POINT('Ctrl Pts',(8.10828546792054,-1.24986760009171,0.682696100760705));
#14321=CARTESIAN_POINT('Ctrl Pts',(8.10985478687837,-1.24981062779486,0.682695370268813));
#14322=CARTESIAN_POINT('Ctrl Pts',(8.11326464342549,-1.24965465239671,0.682715595753076));
#14323=CARTESIAN_POINT('Ctrl Pts',(8.11510409202247,-1.2495501177419,0.682740330911594));
#14324=CARTESIAN_POINT('Ctrl Pts',(8.12014207260669,-1.24920790966494,0.682845651127781));
#14325=CARTESIAN_POINT('Ctrl Pts',(8.12333423895876,-1.24892926854386,0.682953992816581));
#14326=CARTESIAN_POINT('Ctrl Pts',(8.139194120874,-1.2472372768871,0.683691668462565));
#14327=CARTESIAN_POINT('Ctrl Pts',(8.15164141295685,-1.2449338270761,0.684918799511701));
#14328=CARTESIAN_POINT('Ctrl Pts',(8.19196937649467,-1.23428099896052,0.690212518998986));
#14329=CARTESIAN_POINT('Ctrl Pts',(8.21811504697062,-1.22213176592155,0.695755006185672));
#14330=CARTESIAN_POINT('Ctrl Pts',(8.24962874265135,-1.20052913769617,0.699397421419897));
#14331=CARTESIAN_POINT('Ctrl Pts',(8.25758631484639,-1.19433973204149,0.7));
#14332=CARTESIAN_POINT('Ctrl Pts',(8.26514540988519,-1.18768855477586,0.7));
#14333=CARTESIAN_POINT('Origin',(8.1,-1.,0.7));
#14334=CARTESIAN_POINT('Origin',(2.7,1.,0.7));
#14335=CARTESIAN_POINT('',(2.8076286513348,1.22564590451442,0.7));
#14336=CARTESIAN_POINT('',(2.57739843082973,1.21787348447435,0.7));
#14337=CARTESIAN_POINT('Ctrl Pts',(2.80762864495888,1.22564590575571,0.7));
#14338=CARTESIAN_POINT('Ctrl Pts',(2.78743249310418,1.23527907171202,0.7));
#14339=CARTESIAN_POINT('Ctrl Pts',(2.76507271635938,1.24261561512899,0.698430289974852));
#14340=CARTESIAN_POINT('Ctrl Pts',(2.73219941643314,1.24807722603274,0.696876198609429));
#14341=CARTESIAN_POINT('Ctrl Pts',(2.72335305886828,1.24906618730719,0.696525251810408));
#14342=CARTESIAN_POINT('Ctrl Pts',(2.71018695034311,1.24982905432238,0.696188910804419));
#14343=CARTESIAN_POINT('Ctrl Pts',(2.70590779780308,1.24996687586326,0.696107915309552));
#14344=CARTESIAN_POINT('Ctrl Pts',(2.69921702211412,1.25001037316246,0.696030339680738));
#14345=CARTESIAN_POINT('Ctrl Pts',(2.69680890442544,1.24999123464332,0.696012302673685));
#14346=CARTESIAN_POINT('Ctrl Pts',(2.69234597975348,1.24989125947742,0.695997601992606));
#14347=CARTESIAN_POINT('Ctrl Pts',(2.69029169500035,1.24981988388707,0.69599819279703));
#14348=CARTESIAN_POINT('Ctrl Pts',(2.6857660481318,1.24960673159635,0.696015705561832));
#14349=CARTESIAN_POINT('Ctrl Pts',(2.68329599580702,1.24945360531346,0.696035938105249));
#14350=CARTESIAN_POINT('Ctrl Pts',(2.67625328071593,1.24891193026541,0.696123377063474));
#14351=CARTESIAN_POINT('Ctrl Pts',(2.67169109188753,1.24843439216159,0.696216059649547));
#14352=CARTESIAN_POINT('Ctrl Pts',(2.64765560351845,1.24524789167778,0.696873729305584));
#14353=CARTESIAN_POINT('Ctrl Pts',(2.62857598726268,1.24037162800668,0.698048768812303));
#14354=CARTESIAN_POINT('Ctrl Pts',(2.59902076831046,1.22902239593109,0.699541037747764));
#14355=CARTESIAN_POINT('Ctrl Pts',(2.58799157881597,1.22383445108162,0.7));
#14356=CARTESIAN_POINT('Ctrl Pts',(2.57739843082979,1.21787348447436,0.7));
#14357=CARTESIAN_POINT('Origin',(2.7,1.,0.7));
#14358=CARTESIAN_POINT('Origin',(2.7,-1.,0.7));
#14359=CARTESIAN_POINT('',(2.57739843082979,-1.21787348447436,0.7));
#14360=CARTESIAN_POINT('',(2.80762864495888,-1.22564590575571,0.7));
#14361=CARTESIAN_POINT('Ctrl Pts',(2.57739843082979,-1.21787348447436,0.7));
#14362=CARTESIAN_POINT('Ctrl Pts',(2.59689796709118,-1.22884624579732,0.7));
#14363=CARTESIAN_POINT('Ctrl Pts',(2.61871070177046,-1.23767364961455,0.698430520021629));
#14364=CARTESIAN_POINT('Ctrl Pts',(2.6511387549791,-1.24533993869645,0.696876447160353));
#14365=CARTESIAN_POINT('Ctrl Pts',(2.65989793055836,-1.24692336726652,0.696525471319567));
#14366=CARTESIAN_POINT('Ctrl Pts',(2.67298219502323,-1.24857266139659,0.696189053183015));
#14367=CARTESIAN_POINT('Ctrl Pts',(2.67724223626036,-1.24899884484677,0.696108027479433));
#14368=CARTESIAN_POINT('Ctrl Pts',(2.68391475503581,-1.24949361628703,0.696030400846995));
#14369=CARTESIAN_POINT('Ctrl Pts',(2.68631866330158,-1.24963697932539,0.69601234479389));
#14370=CARTESIAN_POINT('Ctrl Pts',(2.69077815115796,-1.24983831390468,0.695997608323079));
#14371=CARTESIAN_POINT('Ctrl Pts',(2.69283257145917,-1.24990568929416,0.695998182544699));
#14372=CARTESIAN_POINT('Ctrl Pts',(2.69736230434386,-1.24999833696454,0.696015659042177));
#14373=CARTESIAN_POINT('Ctrl Pts',(2.69983707579759,-1.25001219669429,0.696035872086962));
#14374=CARTESIAN_POINT('Ctrl Pts',(2.70690037992806,-1.24994687665095,0.696123257636812));
#14375=CARTESIAN_POINT('Ctrl Pts',(2.71148446565418,-1.24977820005943,0.696215908504701));
#14376=CARTESIAN_POINT('Ctrl Pts',(2.73568105999059,-1.24822038288304,0.696873447340259));
#14377=CARTESIAN_POINT('Ctrl Pts',(2.75504695022812,-1.24464213141243,0.698048515307351));
#14378=CARTESIAN_POINT('Ctrl Pts',(2.78530198112344,-1.2353118289445,0.699540950501024));
#14379=CARTESIAN_POINT('Ctrl Pts',(2.79665680001786,-1.23087925931356,0.7));
#14380=CARTESIAN_POINT('Ctrl Pts',(2.80762864495888,-1.22564590575571,0.7));
#14381=CARTESIAN_POINT('Origin',(2.7,-1.,0.7));
#14382=CARTESIAN_POINT('Origin',(8.1,1.,0.7));
#14383=CARTESIAN_POINT('',(8.26514540988519,1.18768855477586,0.7));
#14384=CARTESIAN_POINT('',(7.94916965249954,1.19937453719419,0.7));
#14385=CARTESIAN_POINT('Ctrl Pts',(8.26514540988519,1.18768855477586,0.7));
#14386=CARTESIAN_POINT('Ctrl Pts',(8.24402114884725,1.20627559516199,0.7));
#14387=CARTESIAN_POINT('Ctrl Pts',(8.21930102059268,1.22168408824046,0.695284768760077));
#14388=CARTESIAN_POINT('Ctrl Pts',(8.17833936508797,1.23784683595578,0.688517484674842));
#14389=CARTESIAN_POINT('Ctrl Pts',(8.16442627443898,1.24199461640617,0.686388979601913));
#14390=CARTESIAN_POINT('Ctrl Pts',(8.14282164862934,1.24641910835203,0.684139556285851));
#14391=CARTESIAN_POINT('Ctrl Pts',(8.13541969045672,1.24759243465272,0.683546718614312));
#14392=CARTESIAN_POINT('Ctrl Pts',(8.12445132655127,1.24882623938238,0.682995554842566));
#14393=CARTESIAN_POINT('Ctrl Pts',(8.12094947916695,1.24914555886372,0.68286756899844));
#14394=CARTESIAN_POINT('Ctrl Pts',(8.11555178799172,1.24952297970176,0.682747494033431));
#14395=CARTESIAN_POINT('Ctrl Pts',(8.11366421100955,1.24963346420394,0.682719937279798));
#14396=CARTESIAN_POINT('Ctrl Pts',(8.11020620287515,1.24979651712922,0.682696124556263));
#14397=CARTESIAN_POINT('Ctrl Pts',(8.10863696767328,1.24985569708818,0.682695355189016));
#14398=CARTESIAN_POINT('Ctrl Pts',(8.10522484403353,1.249952190393,0.682715496638402));
#14399=CARTESIAN_POINT('Ctrl Pts',(8.10338263267786,1.24998390529834,0.682740187713169));
#14400=CARTESIAN_POINT('Ctrl Pts',(8.09833277498968,1.25001501472208,0.682845394223802));
#14401=CARTESIAN_POINT('Ctrl Pts',(8.09512844909059,1.24997307323179,0.682953673497893));
#14402=CARTESIAN_POINT('Ctrl Pts',(8.07918314804204,1.24945780552822,0.683691186949858));
#14403=CARTESIAN_POINT('Ctrl Pts',(8.06659630270856,1.24808001426183,0.684918585227095));
#14404=CARTESIAN_POINT('Ctrl Pts',(8.02558960427868,1.24043495378573,0.69021260546313));
#14405=CARTESIAN_POINT('Ctrl Pts',(7.9986188553413,1.2302509517108,0.695754623970086));
#14406=CARTESIAN_POINT('Ctrl Pts',(7.96559475436581,1.21103543221342,0.69939729083119));
#14407=CARTESIAN_POINT('Ctrl Pts',(7.95720051358587,1.20545002552208,0.7));
#14408=CARTESIAN_POINT('Ctrl Pts',(7.94916965151797,1.19937453693185,0.7));
#14409=CARTESIAN_POINT('Origin',(8.1,1.,0.7));
#14410=CARTESIAN_POINT('Ctrl Pts',(1.1,1.14549341399196,0.7));
#14411=CARTESIAN_POINT('Ctrl Pts',(1.89984199608574,1.1957170361627,0.7));
#14412=CARTESIAN_POINT('Ctrl Pts',(2.70080437300401,1.2273695200909,0.7));
#14413=CARTESIAN_POINT('Ctrl Pts',(3.50204003610941,1.24374118183538,0.7));
#14414=CARTESIAN_POINT('Ctrl Pts',(1.09819048660397,1.17431102498992,0.7));
#14415=CARTESIAN_POINT('Ctrl Pts',(1.89847848223077,1.22458382597074,0.70000077422621));
#14416=CARTESIAN_POINT('Ctrl Pts',(2.69984520196781,1.25626413437997,0.699999727319846));
#14417=CARTESIAN_POINT('Ctrl Pts',(3.50144932661635,1.27265074030048,0.700000000000001));
#14418=CARTESIAN_POINT('Ctrl Pts',(1.09505363188407,1.22426736091617,0.676703190608825));
#14419=CARTESIAN_POINT('Ctrl Pts',(1.89610976425884,1.27462253270773,0.67666760713801));
#14420=CARTESIAN_POINT('Ctrl Pts',(2.69818680938115,1.3063522351595,0.67664530655333));
#14421=CARTESIAN_POINT('Ctrl Pts',(3.50042536655637,1.322763754511,0.676632802377821));
#14422=CARTESIAN_POINT('Ctrl Pts',(1.09381704710221,1.24396073223232,0.627109609335854));
#14423=CARTESIAN_POINT('Ctrl Pts',(1.89518106151152,1.29430885982199,0.62701751976321));
#14424=CARTESIAN_POINT('Ctrl Pts',(2.69753328610131,1.32603127467068,0.626959208652505));
#14425=CARTESIAN_POINT('Ctrl Pts',(3.50002334924346,1.34243864233338,0.626926882269943));
#14426=CARTESIAN_POINT('Ctrl Pts',(1.09374258853658,1.24514653057163,0.605486452199395));
#14427=CARTESIAN_POINT('Ctrl Pts',(1.89512529323683,1.29547288309274,0.605377720397184));
#14428=CARTESIAN_POINT('Ctrl Pts',(2.69749615303001,1.32718177535833,0.605308474776761));
#14429=CARTESIAN_POINT('Ctrl Pts',(3.5,1.34358136363184,0.605270327458635));
#14430=CARTESIAN_POINT('',(1.1,1.14549341399195,0.7));
#14431=CARTESIAN_POINT('Ctrl Pts',(1.1,1.14549341399196,0.7));
#14432=CARTESIAN_POINT('Ctrl Pts',(1.59210562457523,1.17639367564078,0.7));
#14433=CARTESIAN_POINT('Ctrl Pts',(2.08463535466703,1.20026407570248,0.7));
#14434=CARTESIAN_POINT('Ctrl Pts',(2.57739190516306,1.2178709162388,0.7));
#14435=CARTESIAN_POINT('',(1.1,1.24553911298206,0.605485603995113));
#14436=CARTESIAN_POINT('Ctrl Pts',(1.1,1.14549341399196,0.7));
#14437=CARTESIAN_POINT('Ctrl Pts',(1.1,1.15341616150799,0.7));
#14438=CARTESIAN_POINT('Ctrl Pts',(1.1000012416168,1.16127613060545,0.699006361583129));
#14439=CARTESIAN_POINT('Ctrl Pts',(1.10000231308998,1.16893252943985,0.697119293189023));
#14440=CARTESIAN_POINT('Ctrl Pts',(1.10000291357081,1.17322337016277,0.696061732044743));
#14441=CARTESIAN_POINT('Ctrl Pts',(1.10000345673767,1.17745032641463,0.694722535963768));
#14442=CARTESIAN_POINT('Ctrl Pts',(1.10000379529503,1.18158693416151,0.693112479763539));
#14443=CARTESIAN_POINT('Ctrl Pts',(1.1000044034764,1.18901789868739,0.690220189452084));
#14444=CARTESIAN_POINT('Ctrl Pts',(1.1000042334852,1.19607766167095,0.686488065947256));
#14445=CARTESIAN_POINT('Ctrl Pts',(1.10000339376692,1.2026196529327,0.681996646156542));
#14446=CARTESIAN_POINT('Ctrl Pts',(1.10000293249552,1.20621327895058,0.67952943359521));
#14447=CARTESIAN_POINT('Ctrl Pts',(1.10000228571683,1.20965039763183,0.676832226278619));
#14448=CARTESIAN_POINT('Ctrl Pts',(1.10000171524363,1.21290279159005,0.673912896410569));
#14449=CARTESIAN_POINT('Ctrl Pts',(1.10000115816795,1.2160788033717,0.671062126739188));
#14450=CARTESIAN_POINT('Ctrl Pts',(1.10000066850715,1.2190594221245,0.668016750164662));
#14451=CARTESIAN_POINT('Ctrl Pts',(1.10000067525152,1.22182202639256,0.664788091882127));
#14452=CARTESIAN_POINT('Ctrl Pts',(1.10000068775799,1.22694487635592,0.658801012170571));
#14453=CARTESIAN_POINT('Ctrl Pts',(1.10000222199399,1.23132099043293,0.652185071179834));
#14454=CARTESIAN_POINT('Ctrl Pts',(1.10000276904041,1.23488987417606,0.64510534613808));
#14455=CARTESIAN_POINT('Ctrl Pts',(1.10000282439334,1.23525099193115,0.644388983656765));
#14456=CARTESIAN_POINT('Ctrl Pts',(1.10000287212626,1.23560380546488,0.64366785367332));
#14457=CARTESIAN_POINT('Ctrl Pts',(1.10000291138002,1.23594822450451,0.642942116631622));
#14458=CARTESIAN_POINT('Ctrl Pts',(1.10000329911404,1.23935026814133,0.635773555081239));
#14459=CARTESIAN_POINT('Ctrl Pts',(1.10000258010782,1.24189771450306,0.628240464257889));
#14460=CARTESIAN_POINT('Ctrl Pts',(1.10000149084855,1.24353681278199,0.620511076118615));
#14461=CARTESIAN_POINT('Ctrl Pts',(1.10000079446814,1.24458471384188,0.615569557890241));
#14462=CARTESIAN_POINT('Ctrl Pts',(1.10000000111128,1.24526049271905,0.610547146027233));
#14463=CARTESIAN_POINT('Ctrl Pts',(1.09999999916631,1.24553911263843,0.605485603997432));
#14464=CARTESIAN_POINT('',(3.5,1.34358136363184,0.605270327458635));
#14465=CARTESIAN_POINT('Ctrl Pts',(3.5,1.34358136363184,0.605270327458635));
#14466=CARTESIAN_POINT('Ctrl Pts',(2.6995848679345,1.32722445934619,0.605308375488923));
#14467=CARTESIAN_POINT('Ctrl Pts',(1.89930203168261,1.29563783986497,0.605377360150118));
#14468=CARTESIAN_POINT('Ctrl Pts',(1.09999999916631,1.24553911263843,0.605485603997431));
#14469=CARTESIAN_POINT('',(3.5,1.24369946473792,0.7));
#14470=CARTESIAN_POINT('Ctrl Pts',(3.5,1.34358136363184,0.605270327458635));
#14471=CARTESIAN_POINT('Ctrl Pts',(3.5,1.34316359984937,0.613184373088104));
#14472=CARTESIAN_POINT('Ctrl Pts',(3.50000057901142,1.34177887744868,0.621008021569537));
#14473=CARTESIAN_POINT('Ctrl Pts',(3.50000082863025,1.33951086762262,0.628580534231506));
#14474=CARTESIAN_POINT('Ctrl Pts',(3.50000096811,1.33824356956914,0.632811834486987));
#14475=CARTESIAN_POINT('Ctrl Pts',(3.50000102536574,1.33669948631919,0.636964759527324));
#14476=CARTESIAN_POINT('Ctrl Pts',(3.50000098105742,1.334886463945,0.641009258704104));
#14477=CARTESIAN_POINT('Ctrl Pts',(3.50000090179773,1.3316432906201,0.648244145614236));
#14478=CARTESIAN_POINT('Ctrl Pts',(3.50000044940971,1.3275777080273,0.655054131048541));
#14479=CARTESIAN_POINT('Ctrl Pts',(3.50000027423476,1.32275302640998,0.661275670751788));
#14480=CARTESIAN_POINT('Ctrl Pts',(3.50000024156065,1.32185311357394,0.66243612938574));
#14481=CARTESIAN_POINT('Ctrl Pts',(3.50000022115524,1.32092666334894,0.663576045687695));
#14482=CARTESIAN_POINT('Ctrl Pts',(3.50000022069074,1.31997391848392,0.664694242102532));
#14483=CARTESIAN_POINT('Ctrl Pts',(3.50000021976176,1.31806844339147,0.666930617752677));
#14484=CARTESIAN_POINT('Ctrl Pts',(3.50000029790302,1.31605782519,0.669080165434128));
#14485=CARTESIAN_POINT('Ctrl Pts',(3.50000040488465,1.31394946763378,0.671139079687271));
#14486=CARTESIAN_POINT('Ctrl Pts',(3.50000069329649,1.3082655455861,0.6766897075128));
#14487=CARTESIAN_POINT('Ctrl Pts',(3.5000011432336,1.30193818666762,0.681521899278667));
#14488=CARTESIAN_POINT('Ctrl Pts',(3.50000129797765,1.29513115062548,0.68558123547136));
#14489=CARTESIAN_POINT('Ctrl Pts',(3.50000139624096,1.2908086457691,0.688158936000333));
#14490=CARTESIAN_POINT('Ctrl Pts',(3.50000139493488,1.28629176508013,0.690424313967808));
#14491=CARTESIAN_POINT('Ctrl Pts',(3.50000129141552,1.28161680488022,0.692354162840695));
#14492=CARTESIAN_POINT('Ctrl Pts',(3.50000112941005,1.27430059661786,0.695374333209024));
#14493=CARTESIAN_POINT('Ctrl Pts',(3.5000007162179,1.26668229982361,0.697540280949125));
#14494=CARTESIAN_POINT('Ctrl Pts',(3.50000038344698,1.25890895215876,0.698782355543395));
#14495=CARTESIAN_POINT('Ctrl Pts',(3.50000016866387,1.25389173534334,0.699584038140014));
#14496=CARTESIAN_POINT('Ctrl Pts',(3.4999999993056,1.24880933504677,0.69999999987784));
#14497=CARTESIAN_POINT('Ctrl Pts',(3.49999999991873,1.24369946470729,0.7));
#14498=CARTESIAN_POINT('Ctrl Pts',(2.80762377174497,1.22564400643366,0.7));
#14499=CARTESIAN_POINT('Ctrl Pts',(3.03837960601223,1.23298334400942,0.7));
#14500=CARTESIAN_POINT('Ctrl Pts',(3.26917843294065,1.23897560812206,0.7));
#14501=CARTESIAN_POINT('Ctrl Pts',(3.49999999991873,1.24369946470729,0.7));
#14502=CARTESIAN_POINT('Ctrl Pts',(7.29709043526678,1.22049830417059,0.7));
#14503=CARTESIAN_POINT('Ctrl Pts',(8.19846709497879,1.19422430779862,0.7));
#14504=CARTESIAN_POINT('Ctrl Pts',(9.09944331332256,1.15544418981837,0.7));
#14505=CARTESIAN_POINT('Ctrl Pts',(10.,1.10900986674273,0.7));
#14506=CARTESIAN_POINT('Ctrl Pts',(7.29793284700474,1.24939875264889,0.7));
#14507=CARTESIAN_POINT('Ctrl Pts',(8.19957769811722,1.22310890030201,0.699999704549177));
#14508=CARTESIAN_POINT('Ctrl Pts',(9.10076698492607,1.18430758604571,0.700000491839571));
#14509=CARTESIAN_POINT('Ctrl Pts',(10.0014871213396,1.13785139984992,0.7));
#14510=CARTESIAN_POINT('Ctrl Pts',(7.29939288958794,1.29948813715084,0.676630595533454));
#14511=CARTESIAN_POINT('Ctrl Pts',(8.20149954052228,1.27317186922949,0.676644146017132));
#14512=CARTESIAN_POINT('Ctrl Pts',(9.10306300621911,1.23433322993607,0.676664155483857));
#14513=CARTESIAN_POINT('Ctrl Pts',(10.0040646682326,1.18784086746588,0.676686753673613));
#14514=CARTESIAN_POINT('Ctrl Pts',(7.29996660609513,1.31917051289423,0.626939603849942));
#14515=CARTESIAN_POINT('Ctrl Pts',(8.20225661204673,1.29285896783792,0.626974637782525));
#14516=CARTESIAN_POINT('Ctrl Pts',(9.10396596140606,1.25402923300358,0.627026849623412));
#14517=CARTESIAN_POINT('Ctrl Pts',(10.0050807923581,1.20754778500352,0.627085325222079));
#14518=CARTESIAN_POINT('Ctrl Pts',(7.29999999953093,1.32031613471704,0.605285370449856));
#14519=CARTESIAN_POINT('Ctrl Pts',(8.20230020786565,1.29401302889245,0.605326714446839));
#14520=CARTESIAN_POINT('Ctrl Pts',(9.10401978846669,1.25519559703033,0.605388684776982));
#14521=CARTESIAN_POINT('Ctrl Pts',(10.0051416645797,1.20872835322339,0.605457722909465));
#14522=CARTESIAN_POINT('',(7.29999999989017,1.22041345054104,0.7));
#14523=CARTESIAN_POINT('Ctrl Pts',(7.29999999978094,1.22041345055303,0.7));
#14524=CARTESIAN_POINT('Ctrl Pts',(7.51641201913776,1.21409884615949,0.7));
#14525=CARTESIAN_POINT('Ctrl Pts',(7.73280095443524,1.20706364503479,0.7));
#14526=CARTESIAN_POINT('Ctrl Pts',(7.94916654146952,1.19937499621344,0.7));
#14527=CARTESIAN_POINT('',(7.29999999953133,1.3203161347307,0.605285370449834));
#14528=CARTESIAN_POINT('Ctrl Pts',(7.29999999989087,1.22041345054982,0.7));
#14529=CARTESIAN_POINT('Ctrl Pts',(7.30000000079355,1.22832360919786,0.699999999740221));
#14530=CARTESIAN_POINT('Ctrl Pts',(7.29999941101664,1.23617007614594,0.699006006469939));
#14531=CARTESIAN_POINT('Ctrl Pts',(7.29999889581476,1.24381267896118,0.697118889344366));
#14532=CARTESIAN_POINT('Ctrl Pts',(7.29999860583198,1.24811433880851,0.696056720321257));
#14533=CARTESIAN_POINT('Ctrl Pts',(7.29999834128398,1.25235147078274,0.694710570513598));
#14534=CARTESIAN_POINT('Ctrl Pts',(7.29999817264931,1.25649739217805,0.693091458416622));
#14535=CARTESIAN_POINT('Ctrl Pts',(7.29999787070862,1.26392067210813,0.690192435210923));
#14536=CARTESIAN_POINT('Ctrl Pts',(7.29999793286912,1.27097116792553,0.686452948287278));
#14537=CARTESIAN_POINT('Ctrl Pts',(7.2999983123982,1.27750284616821,0.681954753865011));
#14538=CARTESIAN_POINT('Ctrl Pts',(7.2999985213788,1.28109939299731,0.679477906983553));
#14539=CARTESIAN_POINT('Ctrl Pts',(7.29999881895966,1.28453837241868,0.676770138671336));
#14540=CARTESIAN_POINT('Ctrl Pts',(7.29999908362886,1.28779148632494,0.673839551409954));
#14541=CARTESIAN_POINT('Ctrl Pts',(7.29999934163235,1.29096267037196,0.670982771155867));
#14542=CARTESIAN_POINT('Ctrl Pts',(7.29999957112158,1.2939379836903,0.667931525418885));
#14543=CARTESIAN_POINT('Ctrl Pts',(7.29999957127586,1.29669488996436,0.664697318929259));
#14544=CARTESIAN_POINT('Ctrl Pts',(7.29999957156178,1.30180432468448,0.658703293276094));
#14545=CARTESIAN_POINT('Ctrl Pts',(7.29999886995656,1.30616650855536,0.652082235935803));
#14546=CARTESIAN_POINT('Ctrl Pts',(7.29999863193158,1.30972187224872,0.644999691185358));
#14547=CARTESIAN_POINT('Ctrl Pts',(7.29999860759325,1.31008541227461,0.644275492840527));
#14548=CARTESIAN_POINT('Ctrl Pts',(7.29999858692673,1.31044047656777,0.643546449710686));
#14549=CARTESIAN_POINT('Ctrl Pts',(7.29999857034625,1.31078697300061,0.642812727646596));
#14550=CARTESIAN_POINT('Ctrl Pts',(7.29999840819729,1.31417553742296,0.635637287305567));
#14551=CARTESIAN_POINT('Ctrl Pts',(7.29999876577208,1.31670951795567,0.628098908385918));
#14552=CARTESIAN_POINT('Ctrl Pts',(7.29999928780719,1.3183355664444,0.620365998324013));
#14553=CARTESIAN_POINT('Ctrl Pts',(7.29999962266353,1.3193785856694,0.615405768714856));
#14554=CARTESIAN_POINT('Ctrl Pts',(7.3,1.32004717656055,0.610364828659741));
#14555=CARTESIAN_POINT('Ctrl Pts',(7.3,1.32031613470337,0.605285370449877));
#14556=CARTESIAN_POINT('',(10.,1.20899340483173,0.605457329065657));
#14557=CARTESIAN_POINT('Ctrl Pts',(9.99999999968202,1.20899340489109,0.605457329065633));
#14558=CARTESIAN_POINT('Ctrl Pts',(9.10058974048747,1.25534320916473,0.605388449123016));
#14559=CARTESIAN_POINT('Ctrl Pts',(8.20058408060299,1.29406305600824,0.605326635812744));
#14560=CARTESIAN_POINT('Ctrl Pts',(7.29999999953093,1.32031613471704,0.605285370449856));
#14561=CARTESIAN_POINT('',(9.99999999523418,1.1090098672342,0.7));
#14562=CARTESIAN_POINT('Ctrl Pts',(9.99999999968202,1.20899340489109,0.605457329065633));
#14563=CARTESIAN_POINT('Ctrl Pts',(9.99999999887489,1.20856043137698,0.613368813757176));
#14564=CARTESIAN_POINT('Ctrl Pts',(9.99999852309337,1.20715974444566,0.621187403383205));
#14565=CARTESIAN_POINT('Ctrl Pts',(9.99999786661901,1.20487567413208,0.628752957409046));
#14566=CARTESIAN_POINT('Ctrl Pts',(9.9999975031266,1.20361097553651,0.63294203403));
#14567=CARTESIAN_POINT('Ctrl Pts',(9.99999733971606,1.20207445367248,0.63705356322819));
#14568=CARTESIAN_POINT('Ctrl Pts',(9.99999742766416,1.20027388348257,0.64105842070465));
#14569=CARTESIAN_POINT('Ctrl Pts',(9.9999975865154,1.19702170610966,0.6482919664668));
#14570=CARTESIAN_POINT('Ctrl Pts',(9.99999868569093,1.19294650045069,0.655099368158521));
#14571=CARTESIAN_POINT('Ctrl Pts',(9.9999991134218,1.18811276085989,0.661317774786376));
#14572=CARTESIAN_POINT('Ctrl Pts',(9.99999919410111,1.18720101282252,0.662490701033652));
#14573=CARTESIAN_POINT('Ctrl Pts',(9.99999924414009,1.18626214680169,0.663642601192937));
#14574=CARTESIAN_POINT('Ctrl Pts',(9.99999924372355,1.18529642131707,0.664772262763739));
#14575=CARTESIAN_POINT('Ctrl Pts',(9.99999924291654,1.18342543943696,0.666960851926287));
#14576=CARTESIAN_POINT('Ctrl Pts',(9.99999905429896,1.18145367213587,0.669066014649603));
#14577=CARTESIAN_POINT('Ctrl Pts',(9.99999879621773,1.17938809187152,0.671084194359814));
#14578=CARTESIAN_POINT('Ctrl Pts',(9.99999808597787,1.17370361260899,0.676638227242868));
#14579=CARTESIAN_POINT('Ctrl Pts',(9.9999969699445,1.16737553754052,0.681473799108647));
#14580=CARTESIAN_POINT('Ctrl Pts',(9.99999660204079,1.16056788011185,0.685537070165577));
#14581=CARTESIAN_POINT('Ctrl Pts',(9.99999636768906,1.15623145667386,0.688125341392612));
#14582=CARTESIAN_POINT('Ctrl Pts',(9.99999638726733,1.15169947441128,0.690399565850749));
#14583=CARTESIAN_POINT('Ctrl Pts',(9.99999666360534,1.14700857532255,0.692336497939236));
#14584=CARTESIAN_POINT('Ctrl Pts',(9.99999709503399,1.13968497812548,0.695360504669253));
#14585=CARTESIAN_POINT('Ctrl Pts',(9.99999815490668,1.13205884654683,0.697530003145419));
#14586=CARTESIAN_POINT('Ctrl Pts',(9.99999900983214,1.12427739544825,0.698775573347137));
#14587=CARTESIAN_POINT('Ctrl Pts',(9.99999956314479,1.11924119569193,0.699581713521624));
#14588=CARTESIAN_POINT('Ctrl Pts',(10.,1.11413933950174,0.7));
#14589=CARTESIAN_POINT('Ctrl Pts',(10.,1.10900986674273,0.7));
#14590=CARTESIAN_POINT('Ctrl Pts',(8.26514054272776,1.18768929227839,0.7));
#14591=CARTESIAN_POINT('Ctrl Pts',(8.84359655063997,1.16547286645366,0.7));
#14592=CARTESIAN_POINT('Ctrl Pts',(9.42188471826001,1.13881853081542,0.7));
#14593=CARTESIAN_POINT('Ctrl Pts',(9.99999999522154,1.10900986698912,0.7));
#14594=CARTESIAN_POINT('Origin',(5.4,-8.11656130105013E-18,0.7));
#14595=CARTESIAN_POINT('',(7.3,-1.22041345053557,0.7));
#14596=CARTESIAN_POINT('Ctrl Pts',(7.94916654049851,-1.19937499624794,0.7));
#14597=CARTESIAN_POINT('Ctrl Pts',(7.73280095382446,-1.20706364505454,0.7));
#14598=CARTESIAN_POINT('Ctrl Pts',(7.51641201888728,-1.21409884616656,0.7));
#14599=CARTESIAN_POINT('Ctrl Pts',(7.29999999989085,-1.22041345054982,0.7));
#14600=CARTESIAN_POINT('',(7.3,-0.712777777777778,0.7));
#14601=CARTESIAN_POINT('',(10.,-1.10900986674244,0.7));
#14602=CARTESIAN_POINT('',(10.,0.653773457742722,0.7));
#14603=CARTESIAN_POINT('Ctrl Pts',(10.,-1.10900986674273,0.7));
#14604=CARTESIAN_POINT('Ctrl Pts',(9.42188472144661,-1.13881853066854,0.7));
#14605=CARTESIAN_POINT('Ctrl Pts',(8.84359655223373,-1.16547286639245,0.7));
#14606=CARTESIAN_POINT('Ctrl Pts',(8.26514054272776,-1.18768929227839,0.7));
#14607=CARTESIAN_POINT('',(7.95,-1.,0.7));
#14608=CARTESIAN_POINT('Origin',(8.1,-1.,0.7));
#14609=CARTESIAN_POINT('',(7.95,1.,0.7));
#14610=CARTESIAN_POINT('Origin',(8.1,1.,0.7));
#14611=CARTESIAN_POINT('',(8.4,-4.89858719658942E-17,0.7));
#14612=CARTESIAN_POINT('Origin',(8.8,0.,0.7));
#14613=CARTESIAN_POINT('Origin',(8.97320508075689,0.3,0.9));
#14614=CARTESIAN_POINT('',(8.97320508075689,0.3,0.9));
#14615=CARTESIAN_POINT('',(9.14641016151377,0.,0.9));
#14616=CARTESIAN_POINT('',(8.59150635094611,0.961121593216771,0.9));
#14617=CARTESIAN_POINT('',(8.97320508075689,0.3,0.6));
#14618=CARTESIAN_POINT('',(8.97320508075689,0.3,0.9));
#14619=CARTESIAN_POINT('',(9.14641016151377,0.,0.6));
#14620=CARTESIAN_POINT('',(9.14641016151377,0.,0.6));
#14621=CARTESIAN_POINT('',(9.14641016151377,0.,0.9));
#14622=CARTESIAN_POINT('Origin',(8.62679491924311,0.3,0.9));
#14623=CARTESIAN_POINT('',(8.62679491924311,0.3,0.9));
#14624=CARTESIAN_POINT('',(7.01339745962156,0.3,0.9));
#14625=CARTESIAN_POINT('',(8.62679491924311,0.3,0.6));
#14626=CARTESIAN_POINT('',(8.62679491924311,0.3,0.9));
#14627=CARTESIAN_POINT('',(8.97320508075689,0.3,0.6));
#14628=CARTESIAN_POINT('Origin',(8.45358983848623,5.55111512312578E-17,
0.9));
#14629=CARTESIAN_POINT('',(8.45358983848623,4.24230095489963E-17,0.9));
#14630=CARTESIAN_POINT('',(8.07189110867545,-0.661121593216771,0.9));
#14631=CARTESIAN_POINT('',(8.45358983848623,5.55111512312578E-17,0.6));
#14632=CARTESIAN_POINT('',(8.45358983848623,4.24230095489963E-17,0.9));
#14633=CARTESIAN_POINT('',(8.62679491924311,0.3,0.6));
#14634=CARTESIAN_POINT('Origin',(8.62679491924311,-0.3,0.9));
#14635=CARTESIAN_POINT('',(8.62679491924311,-0.3,0.9));
#14636=CARTESIAN_POINT('',(8.15849364905389,0.511121593216771,0.9));
#14637=CARTESIAN_POINT('',(8.62679491924311,-0.3,0.6));
#14638=CARTESIAN_POINT('',(8.62679491924311,-0.3,0.9));
#14639=CARTESIAN_POINT('',(8.45358983848623,4.24230095489963E-17,0.6));
#14640=CARTESIAN_POINT('Origin',(8.97320508075689,-0.3,0.9));
#14641=CARTESIAN_POINT('',(8.97320508075689,-0.3,0.9));
#14642=CARTESIAN_POINT('',(7.18660254037844,-0.3,0.9));
#14643=CARTESIAN_POINT('',(8.97320508075689,-0.3,0.6));
#14644=CARTESIAN_POINT('',(8.97320508075689,-0.3,0.9));
#14645=CARTESIAN_POINT('',(8.62679491924311,-0.3,0.6));
#14646=CARTESIAN_POINT('Origin',(9.14641016151377,0.,0.9));
#14647=CARTESIAN_POINT('',(8.67810889132456,-0.811121593216771,0.9));
#14648=CARTESIAN_POINT('',(8.97320508075689,-0.3,0.6));
#14649=CARTESIAN_POINT('Origin',(8.8,5.55111512312578E-17,0.6));
#14650=CARTESIAN_POINT('',(8.63,-2.0818995585505E-17,0.6));
#14651=CARTESIAN_POINT('Origin',(8.8,0.,0.6));
#14652=CARTESIAN_POINT('Origin',(2.17320508075689,0.3,0.9));
#14653=CARTESIAN_POINT('',(2.17320508075689,0.3,0.9));
#14654=CARTESIAN_POINT('',(2.34641016151378,0.,0.9));
#14655=CARTESIAN_POINT('',(2.64150635094611,-0.511121593216773,0.9));
#14656=CARTESIAN_POINT('',(2.17320508075689,0.3,0.6));
#14657=CARTESIAN_POINT('',(2.17320508075689,0.3,0.9));
#14658=CARTESIAN_POINT('',(2.34641016151378,0.,0.6));
#14659=CARTESIAN_POINT('',(2.34641016151378,0.,0.6));
#14660=CARTESIAN_POINT('',(2.34641016151378,0.,0.9));
#14661=CARTESIAN_POINT('Origin',(1.82679491924311,0.3,0.9));
#14662=CARTESIAN_POINT('',(1.82679491924311,0.3,0.9));
#14663=CARTESIAN_POINT('',(3.61339745962156,0.3,0.9));
#14664=CARTESIAN_POINT('',(1.82679491924311,0.3,0.6));
#14665=CARTESIAN_POINT('',(1.82679491924311,0.3,0.9));
#14666=CARTESIAN_POINT('',(2.17320508075689,0.3,0.6));
#14667=CARTESIAN_POINT('Origin',(1.65358983848622,5.55111512312578E-17,
0.9));
#14668=CARTESIAN_POINT('',(1.65358983848622,4.24230095489963E-17,0.9));
#14669=CARTESIAN_POINT('',(2.12189110867545,0.811121593216773,0.9));
#14670=CARTESIAN_POINT('',(1.65358983848622,5.55111512312578E-17,0.6));
#14671=CARTESIAN_POINT('',(1.65358983848622,4.24230095489963E-17,0.9));
#14672=CARTESIAN_POINT('',(1.82679491924311,0.3,0.6));
#14673=CARTESIAN_POINT('Origin',(1.82679491924311,-0.3,0.9));
#14674=CARTESIAN_POINT('',(1.82679491924311,-0.3,0.9));
#14675=CARTESIAN_POINT('',(2.20849364905389,-0.961121593216772,0.9));
#14676=CARTESIAN_POINT('',(1.82679491924311,-0.3,0.6));
#14677=CARTESIAN_POINT('',(1.82679491924311,-0.3,0.9));
#14678=CARTESIAN_POINT('',(1.65358983848622,4.24230095489963E-17,0.6));
#14679=CARTESIAN_POINT('Origin',(2.17320508075689,-0.3,0.9));
#14680=CARTESIAN_POINT('',(2.17320508075689,-0.3,0.9));
#14681=CARTESIAN_POINT('',(3.78660254037844,-0.3,0.9));
#14682=CARTESIAN_POINT('',(2.17320508075689,-0.3,0.6));
#14683=CARTESIAN_POINT('',(2.17320508075689,-0.3,0.9));
#14684=CARTESIAN_POINT('',(1.82679491924311,-0.3,0.6));
#14685=CARTESIAN_POINT('Origin',(2.34641016151378,0.,0.9));
#14686=CARTESIAN_POINT('',(2.72810889132455,0.661121593216773,0.9));
#14687=CARTESIAN_POINT('',(2.17320508075689,-0.3,0.6));
#14688=CARTESIAN_POINT('Origin',(2.,5.55111512312578E-17,0.6));
#14689=CARTESIAN_POINT('',(1.83,-2.0818995585505E-17,0.6));
#14690=CARTESIAN_POINT('Origin',(2.,0.,0.6));
#14691=CARTESIAN_POINT('Origin',(8.1,-1.,0.8));
#14692=CARTESIAN_POINT('',(7.95,-1.,0.9));
#14693=CARTESIAN_POINT('Origin',(8.1,-1.,0.9));
#14694=CARTESIAN_POINT('',(7.95,-1.,0.8));
#14695=CARTESIAN_POINT('Origin',(2.7,-1.,0.8));
#14696=CARTESIAN_POINT('',(2.55,-1.,0.9));
#14697=CARTESIAN_POINT('Origin',(2.7,-1.,0.9));
#14698=CARTESIAN_POINT('',(2.55,-1.,0.7));
#14699=CARTESIAN_POINT('',(2.55,-1.,0.8));
#14700=CARTESIAN_POINT('Origin',(2.7,-1.,0.7));
#14701=CARTESIAN_POINT('Origin',(2.7,1.,0.8));
#14702=CARTESIAN_POINT('',(2.55,1.,0.9));
#14703=CARTESIAN_POINT('Origin',(2.7,1.,0.9));
#14704=CARTESIAN_POINT('',(2.55,1.,0.7));
#14705=CARTESIAN_POINT('',(2.55,1.,0.8));
#14706=CARTESIAN_POINT('Origin',(2.7,1.,0.7));
#14707=CARTESIAN_POINT('Origin',(8.1,1.,0.8));
#14708=CARTESIAN_POINT('',(7.95,1.,0.9));
#14709=CARTESIAN_POINT('Origin',(8.1,1.,0.9));
#14710=CARTESIAN_POINT('',(7.95,1.,0.8));
#14711=CARTESIAN_POINT('Origin',(2.,0.,0.45));
#14712=CARTESIAN_POINT('',(1.83,-2.0818995585505E-17,0.32));
#14713=CARTESIAN_POINT('',(1.83,2.0818995585505E-17,0.45));
#14714=CARTESIAN_POINT('Origin',(2.,0.,0.32));
#14715=CARTESIAN_POINT('Origin',(8.8,0.,0.45));
#14716=CARTESIAN_POINT('',(8.63,-2.0818995585505E-17,0.32));
#14717=CARTESIAN_POINT('',(8.63,2.0818995585505E-17,0.45));
#14718=CARTESIAN_POINT('Origin',(8.8,0.,0.32));
#14719=CARTESIAN_POINT('Origin',(10.,-0.62,0.32));
#14720=CARTESIAN_POINT('',(0.200274469199584,-0.62,0.));
#14721=CARTESIAN_POINT('',(0.217044958570157,-0.62,0.32));
#14722=CARTESIAN_POINT('',(0.221783445591644,-0.62,0.410415718550007));
#14723=CARTESIAN_POINT('',(0.,-0.62,0.));
#14724=CARTESIAN_POINT('',(7.7,-0.62,0.));
#14725=CARTESIAN_POINT('',(0.0167704893705732,-0.62,0.32));
#14726=CARTESIAN_POINT('',(0.0220575386407278,-0.62,0.420882909798596));
#14727=CARTESIAN_POINT('',(-0.1,-0.62,0.32));
#14728=CARTESIAN_POINT('Origin',(10.,-0.62,0.32));
#14729=CARTESIAN_POINT('',(0.9,-0.62,0.32));
#14730=CARTESIAN_POINT('',(0.9,-0.62,0.));
#14731=CARTESIAN_POINT('',(0.9,-0.62,0.16));
#14732=CARTESIAN_POINT('',(1.1,-0.62,0.32));
#14733=CARTESIAN_POINT('',(-0.1,-0.62,0.32));
#14734=CARTESIAN_POINT('',(1.1,-0.62,0.));
#14735=CARTESIAN_POINT('',(1.1,-0.62,0.16));
#14736=CARTESIAN_POINT('',(7.7,-0.62,0.));
#14737=CARTESIAN_POINT('Origin',(10.,-0.62,0.32));
#14738=CARTESIAN_POINT('',(3.5,-0.62,0.32));
#14739=CARTESIAN_POINT('',(3.5,-0.62,0.));
#14740=CARTESIAN_POINT('',(3.5,-0.62,0.16));
#14741=CARTESIAN_POINT('',(3.7,-0.62,0.32));
#14742=CARTESIAN_POINT('',(-0.1,-0.62,0.32));
#14743=CARTESIAN_POINT('',(3.7,-0.62,0.));
#14744=CARTESIAN_POINT('',(3.7,-0.62,0.16));
#14745=CARTESIAN_POINT('',(7.7,-0.62,0.));
#14746=CARTESIAN_POINT('Origin',(10.,-0.62,0.32));
#14747=CARTESIAN_POINT('',(7.1,-0.62,0.32));
#14748=CARTESIAN_POINT('',(7.1,-0.62,0.));
#14749=CARTESIAN_POINT('',(7.1,-0.62,0.16));
#14750=CARTESIAN_POINT('',(7.3,-0.62,0.32));
#14751=CARTESIAN_POINT('',(-0.1,-0.62,0.32));
#14752=CARTESIAN_POINT('',(7.3,-0.62,0.));
#14753=CARTESIAN_POINT('',(7.3,-0.62,0.16));
#14754=CARTESIAN_POINT('',(7.7,-0.62,0.));
#14755=CARTESIAN_POINT('Origin',(-0.0999999999999996,0.62,0.32));
#14756=CARTESIAN_POINT('',(0.217044958570158,0.62,0.32));
#14757=CARTESIAN_POINT('',(0.200274469199584,0.62,0.));
#14758=CARTESIAN_POINT('',(0.207951231396534,0.62,0.146481348799182));
#14759=CARTESIAN_POINT('',(0.0167704893705736,0.62,0.32));
#14760=CARTESIAN_POINT('',(10.,0.62,0.32));
#14761=CARTESIAN_POINT('',(0.,0.62,0.));
#14762=CARTESIAN_POINT('',(0.00822532444561912,0.62,0.156948540047771));
#14763=CARTESIAN_POINT('',(2.65,0.62,0.));
#14764=CARTESIAN_POINT('Origin',(-0.0999999999999996,0.62,0.32));
#14765=CARTESIAN_POINT('',(0.9,0.62,0.));
#14766=CARTESIAN_POINT('',(0.9,0.62,0.32));
#14767=CARTESIAN_POINT('',(0.9,0.62,0.16));
#14768=CARTESIAN_POINT('',(1.1,0.62,0.));
#14769=CARTESIAN_POINT('',(2.65,0.62,0.));
#14770=CARTESIAN_POINT('',(1.1,0.62,0.32));
#14771=CARTESIAN_POINT('',(1.1,0.62,0.16));
#14772=CARTESIAN_POINT('',(10.,0.62,0.32));
#14773=CARTESIAN_POINT('Origin',(-0.0999999999999996,0.62,0.32));
#14774=CARTESIAN_POINT('',(3.5,0.62,0.));
#14775=CARTESIAN_POINT('',(3.5,0.62,0.32));
#14776=CARTESIAN_POINT('',(3.5,0.62,0.16));
#14777=CARTESIAN_POINT('',(3.7,0.62,0.));
#14778=CARTESIAN_POINT('',(2.65,0.62,0.));
#14779=CARTESIAN_POINT('',(3.7,0.62,0.32));
#14780=CARTESIAN_POINT('',(3.7,0.62,0.16));
#14781=CARTESIAN_POINT('',(10.,0.62,0.32));
#14782=CARTESIAN_POINT('Origin',(4.95,0.,0.32));
#14783=CARTESIAN_POINT('',(1.6,-4.89858719658941E-17,0.32));
#14784=CARTESIAN_POINT('Origin',(2.,0.,0.32));
#14785=CARTESIAN_POINT('Origin',(4.95,0.,0.32));
#14786=CARTESIAN_POINT('',(8.4,-4.89858719658942E-17,0.32));
#14787=CARTESIAN_POINT('Origin',(8.8,0.,0.32));
#14788=CARTESIAN_POINT('Origin',(4.95,0.,0.32));
#14789=CARTESIAN_POINT('',(0.217044958570157,-0.7,0.32));
#14790=CARTESIAN_POINT('',(0.0167704893705731,-0.7,0.32));
#14791=CARTESIAN_POINT('Origin',(4.95,0.,0.32));
#14792=CARTESIAN_POINT('',(0.9,0.671641708581009,0.32));
#14793=CARTESIAN_POINT('',(1.1,-0.671641708581009,0.32));
#14794=CARTESIAN_POINT('Origin',(4.95,0.,0.32));
#14795=CARTESIAN_POINT('',(3.5,0.723888888888889,0.32));
#14796=CARTESIAN_POINT('',(3.7,-0.723888888888889,0.32));
#14797=CARTESIAN_POINT('Origin',(4.95,0.,0.32));
#14798=CARTESIAN_POINT('',(7.1,0.62,0.32));
#14799=CARTESIAN_POINT('',(7.1,0.712777777777778,0.32));
#14800=CARTESIAN_POINT('',(7.3,0.62,0.32));
#14801=CARTESIAN_POINT('',(10.,0.62,0.32));
#14802=CARTESIAN_POINT('',(7.3,-0.712777777777778,0.32));
#14803=CARTESIAN_POINT('Origin',(-0.0999999999999996,0.62,0.32));
#14804=CARTESIAN_POINT('',(7.1,0.62,0.));
#14805=CARTESIAN_POINT('',(7.1,0.62,0.16));
#14806=CARTESIAN_POINT('',(7.3,0.62,0.));
#14807=CARTESIAN_POINT('',(2.65,0.62,0.));
#14808=CARTESIAN_POINT('',(7.3,0.62,0.16));
#14809=CARTESIAN_POINT('Origin',(10.,1.30754691548544,0.));
#14810=CARTESIAN_POINT('',(10.,1.24211782565704,0.));
#14811=CARTESIAN_POINT('',(10.,-1.24211782565704,0.));
#14812=CARTESIAN_POINT('',(10.,1.30754691548544,0.));
#14813=CARTESIAN_POINT('',(10.,-1.20899340483173,0.605457329065657));
#14814=CARTESIAN_POINT('Ctrl Pts',(10.,-1.20899340483173,0.605457329065657));
#14815=CARTESIAN_POINT('Ctrl Pts',(10.,-1.21451837038612,0.504502771559899));
#14816=CARTESIAN_POINT('Ctrl Pts',(10.,-1.22004249263249,0.403547366186347));
#14817=CARTESIAN_POINT('Ctrl Pts',(10.,-1.23108392958594,0.201728789021226));
#14818=CARTESIAN_POINT('Ctrl Pts',(10.,-1.23660133320922,0.100864020914724));
#14819=CARTESIAN_POINT('Ctrl Pts',(10.,-1.24211782565704,0.));
#14820=CARTESIAN_POINT('Ctrl Pts',(10.,-1.10900986674273,0.7));
#14821=CARTESIAN_POINT('Ctrl Pts',(10.,-1.11692706738765,0.7));
#14822=CARTESIAN_POINT('Ctrl Pts',(9.99999896020971,-1.12478097169818,0.699006158364426));
#14823=CARTESIAN_POINT('Ctrl Pts',(9.99999805494427,-1.13243115645175,0.697118998397561));
#14824=CARTESIAN_POINT('Ctrl Pts',(9.99999754769332,-1.13671781459207,0.696061558623929));
#14825=CARTESIAN_POINT('Ctrl Pts',(9.99999708556116,-1.14094056283945,0.694722610426682));
#14826=CARTESIAN_POINT('Ctrl Pts',(9.99999679002998,-1.14507302265453,0.693112977943955));
#14827=CARTESIAN_POINT('Ctrl Pts',(9.99999625879002,-1.15250143622127,0.690219540062595));
#14828=CARTESIAN_POINT('Ctrl Pts',(9.999996365957,-1.15955821040664,0.686485807665162));
#14829=CARTESIAN_POINT('Ctrl Pts',(9.99999703387985,-1.16609707610076,0.681992895329386));
#14830=CARTESIAN_POINT('Ctrl Pts',(9.99999740034986,-1.16968476316425,0.679527763880215));
#14831=CARTESIAN_POINT('Ctrl Pts',(9.99999792190556,-1.17311627083768,0.676833210412541));
#14832=CARTESIAN_POINT('Ctrl Pts',(9.99999838578331,-1.17636354905877,0.673917165661822));
#14833=CARTESIAN_POINT('Ctrl Pts',(9.99999884023993,-1.17954487655573,0.671060344436104));
#14834=CARTESIAN_POINT('Ctrl Pts',(9.99999924462882,-1.18253006594632,0.668008218820746));
#14835=CARTESIAN_POINT('Ctrl Pts',(9.99999924442301,-1.185296421281,0.664772262763763));
#14836=CARTESIAN_POINT('Ctrl Pts',(9.99999924404215,-1.19041578560695,0.658783864313737));
#14837=CARTESIAN_POINT('Ctrl Pts',(9.99999800949836,-1.19478865237554,0.652167294255586));
#14838=CARTESIAN_POINT('Ctrl Pts',(9.99999759228052,-1.19835462180986,0.645087621913151));
#14839=CARTESIAN_POINT('Ctrl Pts',(9.99999755030119,-1.19871341999785,0.644375284453517));
#14840=CARTESIAN_POINT('Ctrl Pts',(9.9999975145836,-1.19906401030029,0.643658239626438));
#14841=CARTESIAN_POINT('Ctrl Pts',(9.99999748581823,-1.19940630408966,0.642936645100882));
#14842=CARTESIAN_POINT('Ctrl Pts',(9.99999720003888,-1.20280693749908,0.635767720253638));
#14843=CARTESIAN_POINT('Ctrl Pts',(9.9999978299417,-1.20535324884233,0.628234501710241));
#14844=CARTESIAN_POINT('Ctrl Pts',(9.99999874867777,-1.20699142055415,0.62050509267719));
#14845=CARTESIAN_POINT('Ctrl Pts',(9.99999933690345,-1.20804026874419,0.615556297251186));
#14846=CARTESIAN_POINT('Ctrl Pts',(9.99999999916487,-1.20871598809812,0.61052641213707));
#14847=CARTESIAN_POINT('Ctrl Pts',(9.99999999968202,-1.20899340489109,0.605457329065633));
#14848=CARTESIAN_POINT('Ctrl Pts',(10.,1.24211782565704,0.));
#14849=CARTESIAN_POINT('Ctrl Pts',(10.,1.23660053043673,0.100878698875723));
#14850=CARTESIAN_POINT('Ctrl Pts',(10.,1.23108232376984,0.201758145268796));
#14851=CARTESIAN_POINT('Ctrl Pts',(10.,1.22004088630648,0.403576722396156));
#14852=CARTESIAN_POINT('Ctrl Pts',(10.,1.2145175671044,0.504517449470448));
#14853=CARTESIAN_POINT('Ctrl Pts',(10.,1.20899340483173,0.605457329065657));
#14854=CARTESIAN_POINT('Origin',(7.3,-1.42555555555556,0.));
#14855=CARTESIAN_POINT('',(7.3,1.35236351479115,0.));
#14856=CARTESIAN_POINT('',(7.3,-1.42555555555556,0.));
#14857=CARTESIAN_POINT('Ctrl Pts',(7.29999999953133,1.3203161347307,0.605285370449834));
#14858=CARTESIAN_POINT('Ctrl Pts',(7.29999999953133,1.32565322760551,0.504490726585133));
#14859=CARTESIAN_POINT('Ctrl Pts',(7.3,1.33099015509697,0.403695123734478));
#14860=CARTESIAN_POINT('Ctrl Pts',(7.3,1.34167258064689,0.201933969199042));
#14861=CARTESIAN_POINT('Ctrl Pts',(7.3,1.34701817868136,0.100966514951419));
#14862=CARTESIAN_POINT('Ctrl Pts',(7.3,1.35236351479115,0.));
#14863=CARTESIAN_POINT('',(7.29999999953133,-1.3203161347307,0.605285370449834));
#14864=CARTESIAN_POINT('Ctrl Pts',(7.3,-1.32031613470337,0.605285370449877));
#14865=CARTESIAN_POINT('Ctrl Pts',(7.3,-1.31989712778929,0.61319860217968));
#14866=CARTESIAN_POINT('Ctrl Pts',(7.29999916171872,-1.31851071739963,0.621020829077898));
#14867=CARTESIAN_POINT('Ctrl Pts',(7.29999878808195,-1.31624092632926,0.628591660945423));
#14868=CARTESIAN_POINT('Ctrl Pts',(7.29999857947278,-1.31497365483497,0.632818613610392));
#14869=CARTESIAN_POINT('Ctrl Pts',(7.29999848639856,-1.31343001415,0.636967235874856));
#14870=CARTESIAN_POINT('Ctrl Pts',(7.29999853830689,-1.31161789606625,0.641007613679984));
#14871=CARTESIAN_POINT('Ctrl Pts',(7.29999863125487,-1.30837308502546,0.648242386418365));
#14872=CARTESIAN_POINT('Ctrl Pts',(7.29999925734287,-1.30430566789097,0.655052076019481));
#14873=CARTESIAN_POINT('Ctrl Pts',(7.29999949821933,-1.29947941328181,0.661273460789274));
#14874=CARTESIAN_POINT('Ctrl Pts',(7.29999954322,-1.29857776968225,0.662435743389828));
#14875=CARTESIAN_POINT('Ctrl Pts',(7.29999957102613,-1.29764951297213,0.663577423078133));
#14876=CARTESIAN_POINT('Ctrl Pts',(7.2999995707084,-1.29669488998092,0.664697318929248));
#14877=CARTESIAN_POINT('Ctrl Pts',(7.29999957007561,-1.29479368240016,0.666927680549918));
#14878=CARTESIAN_POINT('Ctrl Pts',(7.29999945886743,-1.29278792931167,0.669071688571899));
#14879=CARTESIAN_POINT('Ctrl Pts',(7.29999930790078,-1.2906849717248,0.671125563583336));
#14880=CARTESIAN_POINT('Ctrl Pts',(7.29999889984047,-1.28500071247856,0.676677153447665));
#14881=CARTESIAN_POINT('Ctrl Pts',(7.29999826931494,-1.27867319504519,0.681510485910933));
#14882=CARTESIAN_POINT('Ctrl Pts',(7.29999806345125,-1.27186607945067,0.685571085769401));
#14883=CARTESIAN_POINT('Ctrl Pts',(7.29999793266427,-1.26754145993833,0.688150820039508));
#14884=CARTESIAN_POINT('Ctrl Pts',(7.29999794545359,-1.26302231037287,0.690417984675215));
#14885=CARTESIAN_POINT('Ctrl Pts',(7.29999810371711,-1.25834494218995,0.69234933099425));
#14886=CARTESIAN_POINT('Ctrl Pts',(7.29999835129001,-1.25102809722258,0.695370551698293));
#14887=CARTESIAN_POINT('Ctrl Pts',(7.29999895574222,-1.24340909242398,0.6975375590939));
#14888=CARTESIAN_POINT('Ctrl Pts',(7.29999944081525,-1.2356348173965,0.698780605629559));
#14889=CARTESIAN_POINT('Ctrl Pts',(7.29999975409932,-1.23061380764338,0.699583426311495));
#14890=CARTESIAN_POINT('Ctrl Pts',(7.30000000047446,-1.22552743956586,0.699999999832051));
#14891=CARTESIAN_POINT('Ctrl Pts',(7.29999999989087,-1.22041345054982,0.7));
#14892=CARTESIAN_POINT('',(7.3,-1.35236351479115,0.));
#14893=CARTESIAN_POINT('Ctrl Pts',(7.3,-1.35236351479115,0.));
#14894=CARTESIAN_POINT('Ctrl Pts',(7.3,-1.34701814920095,0.100967071798286));
#14895=CARTESIAN_POINT('Ctrl Pts',(7.3,-1.34167252169398,0.201935082699409));
#14896=CARTESIAN_POINT('Ctrl Pts',(7.3,-1.33099009614589,0.403696237111114));
#14897=CARTESIAN_POINT('Ctrl Pts',(7.29999999953133,-1.32565319812959,0.504491283257837));
#14898=CARTESIAN_POINT('Ctrl Pts',(7.29999999953133,-1.3203161347307,0.605285370449834));
#14899=CARTESIAN_POINT('',(7.3,-1.42555555555556,0.));
#14900=CARTESIAN_POINT('Origin',(3.7,-1.44777777777778,0.));
#14901=CARTESIAN_POINT('',(3.7,1.37924639543935,0.));
#14902=CARTESIAN_POINT('',(3.7,-1.44777777777778,0.));
#14903=CARTESIAN_POINT('',(3.7,1.34735368793805,0.605261457205193));
#14904=CARTESIAN_POINT('Ctrl Pts',(3.7,1.34735368793805,0.605261457205193));
#14905=CARTESIAN_POINT('Ctrl Pts',(3.7,1.35266395147774,0.504488703431434));
#14906=CARTESIAN_POINT('Ctrl Pts',(3.7,1.35797406404029,0.40371594170176));
#14907=CARTESIAN_POINT('Ctrl Pts',(3.7,1.36860496587027,0.201962122597264));
#14908=CARTESIAN_POINT('Ctrl Pts',(3.7,1.37392575452088,0.100981065191366));
#14909=CARTESIAN_POINT('Ctrl Pts',(3.7,1.37924639543935,0.));
#14910=CARTESIAN_POINT('',(3.7,1.24747724070879,0.7));
#14911=CARTESIAN_POINT('Ctrl Pts',(3.7,1.24747724070879,0.7));
#14912=CARTESIAN_POINT('Ctrl Pts',(3.7,1.25538532734776,0.7));
#14913=CARTESIAN_POINT('Ctrl Pts',(3.70000034866643,1.26322972530331,0.699006048248363));
#14914=CARTESIAN_POINT('Ctrl Pts',(3.70000065268588,1.27087026624727,0.697119044026295));
#14915=CARTESIAN_POINT('Ctrl Pts',(3.7000008238479,1.27517186762995,0.696056666371322));
#14916=CARTESIAN_POINT('Ctrl Pts',(3.70000097972585,1.27940891103121,0.694710185093394));
#14917=CARTESIAN_POINT('Ctrl Pts',(3.70000107833511,1.28355469746902,0.693090631030141));
#14918=CARTESIAN_POINT('Ctrl Pts',(3.70000125487464,1.29097687270382,0.690191153635441));
#14919=CARTESIAN_POINT('Ctrl Pts',(3.7000012145424,1.29802606517866,0.686451118058958));
#14920=CARTESIAN_POINT('Ctrl Pts',(3.70000098691147,1.3045562506385,0.681952404110064));
#14921=CARTESIAN_POINT('Ctrl Pts',(3.70000086156653,1.30815209635338,0.679475187900035));
#14922=CARTESIAN_POINT('Ctrl Pts',(3.70000068390876,1.31159030769532,0.676767042898431));
#14923=CARTESIAN_POINT('Ctrl Pts',(3.70000052608992,1.31484259178137,0.673836088143417));
#14924=CARTESIAN_POINT('Ctrl Pts',(3.70000037216713,1.31801458722906,0.670977489418868));
#14925=CARTESIAN_POINT('Ctrl Pts',(3.70000023558528,1.32099045552882,0.667924239810466));
#14926=CARTESIAN_POINT('Ctrl Pts',(3.70000023595245,1.32374763345498,0.664687876924229));
#14927=CARTESIAN_POINT('Ctrl Pts',(3.70000023663259,1.32885491153898,0.658692977181302));
#14928=CARTESIAN_POINT('Ctrl Pts',(3.70000065621025,1.33321474659758,0.652071180203097));
#14929=CARTESIAN_POINT('Ctrl Pts',(3.70000080093706,1.33676785491319,0.644988218508662));
#14930=CARTESIAN_POINT('Ctrl Pts',(3.70000081573428,1.33713113341147,0.644264039153811));
#14931=CARTESIAN_POINT('Ctrl Pts',(3.70000082835625,1.33748593861467,0.643535019157411));
#14932=CARTESIAN_POINT('Ctrl Pts',(3.70000083855542,1.33783217873901,0.642801324492746));
#14933=CARTESIAN_POINT('Ctrl Pts',(3.70000093832019,1.34121897990539,0.63562457699476));
#14934=CARTESIAN_POINT('Ctrl Pts',(3.70000072997693,1.34375116782692,0.628085030530103));
#14935=CARTESIAN_POINT('Ctrl Pts',(3.70000042189378,1.34537558692779,0.6203512574804));
#14936=CARTESIAN_POINT('Ctrl Pts',(3.70000022417294,1.3464181026242,0.615387895628485));
#14937=CARTESIAN_POINT('Ctrl Pts',(3.70000000036652,1.34708586836718,0.6103438638189));
#14938=CARTESIAN_POINT('Ctrl Pts',(3.69999999992214,1.34735368792773,0.6052614572053));
#14939=CARTESIAN_POINT('',(3.7,-1.24747724070944,0.7));
#14940=CARTESIAN_POINT('',(3.7,-0.723888888888889,0.7));
#14941=CARTESIAN_POINT('',(3.7,-1.34735368793805,0.605261457205193));
#14942=CARTESIAN_POINT('Ctrl Pts',(3.69999999992215,-1.34735368792773,0.6052614572053));
#14943=CARTESIAN_POINT('Ctrl Pts',(3.70000000061408,-1.34693666923469,0.613175212866596));
#14944=CARTESIAN_POINT('Ctrl Pts',(3.70000049671034,-1.34555248374866,0.620998392122869));
#14945=CARTESIAN_POINT('Ctrl Pts',(3.70000071566022,-1.34328499565267,0.628570462735333));
#14946=CARTESIAN_POINT('Ctrl Pts',(3.70000083807517,-1.34201724238155,0.632804009674372));
#14947=CARTESIAN_POINT('Ctrl Pts',(3.7000008913247,-1.34047237297042,0.63695909738719));
#14948=CARTESIAN_POINT('Ctrl Pts',(3.70000085837557,-1.33865827982058,0.641005656934072));
#14949=CARTESIAN_POINT('Ctrl Pts',(3.7000007994669,-1.33541492172585,0.648240369034365));
#14950=CARTESIAN_POINT('Ctrl Pts',(3.70000042420685,-1.33134915897915,0.655050234746405));
#14951=CARTESIAN_POINT('Ctrl Pts',(3.70000027984635,-1.32652447879733,0.661271863919233));
#14952=CARTESIAN_POINT('Ctrl Pts',(3.70000025294096,-1.32562527203035,0.662431429080655));
#14953=CARTESIAN_POINT('Ctrl Pts',(3.7000002362737,-1.32469957579387,0.663570491348455));
#14954=CARTESIAN_POINT('Ctrl Pts',(3.70000023630138,-1.32374763346102,0.664687876924223));
#14955=CARTESIAN_POINT('Ctrl Pts',(3.70000023635686,-1.32184039796576,0.666926581264246));
#14956=CARTESIAN_POINT('Ctrl Pts',(3.70000030283857,-1.31982784222224,0.669078323867587));
#14957=CARTESIAN_POINT('Ctrl Pts',(3.70000039320883,-1.31771738411303,0.671139279696989));
#14958=CARTESIAN_POINT('Ctrl Pts',(3.70000063660146,-1.3120333248939,0.676690015307994));
#14959=CARTESIAN_POINT('Ctrl Pts',(3.7000010126336,-1.30570602994251,0.681522474044465));
#14960=CARTESIAN_POINT('Ctrl Pts',(3.70000113724274,-1.29889910811053,0.685582059356066));
#14961=CARTESIAN_POINT('Ctrl Pts',(3.70000121634872,-1.29457784995583,0.688159217808216));
#14962=CARTESIAN_POINT('Ctrl Pts',(3.70000121058612,-1.2900623422215,0.690424215862126));
#14963=CARTESIAN_POINT('Ctrl Pts',(3.70000111831253,-1.28538881676413,0.692353818784707));
#14964=CARTESIAN_POINT('Ctrl Pts',(3.70000097388434,-1.27807373536961,0.695374066040565));
#14965=CARTESIAN_POINT('Ctrl Pts',(3.70000061691996,-1.27045659963863,0.697540160564298));
#14966=CARTESIAN_POINT('Ctrl Pts',(3.7000003304055,-1.26268427129293,0.698782316368755));
#14967=CARTESIAN_POINT('Ctrl Pts',(3.70000014548661,-1.25766794365683,0.699584014420239));
#14968=CARTESIAN_POINT('Ctrl Pts',(3.7,-1.25258637988459,0.7));
#14969=CARTESIAN_POINT('Ctrl Pts',(3.7,-1.24747724070879,0.7));
#14970=CARTESIAN_POINT('',(3.7,-1.37924639543935,0.));
#14971=CARTESIAN_POINT('Ctrl Pts',(3.7,-1.37924639543935,0.));
#14972=CARTESIAN_POINT('Ctrl Pts',(3.7,-1.37392574223662,0.100981298335747));
#14973=CARTESIAN_POINT('Ctrl Pts',(3.7,-1.36860494130098,0.201962588887634));
#14974=CARTESIAN_POINT('Ctrl Pts',(3.7,-1.35797403946962,0.403716407992068));
#14975=CARTESIAN_POINT('Ctrl Pts',(3.7,-1.3526639391921,0.504488936575732));
#14976=CARTESIAN_POINT('Ctrl Pts',(3.7,-1.34735368793805,0.605261457205193));
#14977=CARTESIAN_POINT('',(3.7,-1.44777777777778,0.));
#14978=CARTESIAN_POINT('Origin',(1.1,-1.34328341716202,0.));
#14979=CARTESIAN_POINT('',(1.1,1.27885335043294,0.));
#14980=CARTESIAN_POINT('',(1.1,-1.34328341716202,0.));
#14981=CARTESIAN_POINT('Ctrl Pts',(1.1,1.24553911298206,0.605485603995113));
#14982=CARTESIAN_POINT('Ctrl Pts',(1.1,1.25109559382646,0.504544105903265));
#14983=CARTESIAN_POINT('Ctrl Pts',(1.1,1.25665083308595,0.403601248768354));
#14984=CARTESIAN_POINT('Ctrl Pts',(1.1,1.26775551906787,0.201773573764085));
#14985=CARTESIAN_POINT('Ctrl Pts',(1.1,1.2733051088238,0.100886182270816));
#14986=CARTESIAN_POINT('Ctrl Pts',(1.1,1.27885335043294,0.));
#14987=CARTESIAN_POINT('',(1.1,-1.14549341399195,0.7));
#14988=CARTESIAN_POINT('',(1.1,-0.671641708581009,0.7));
#14989=CARTESIAN_POINT('',(1.1,-1.24553911298206,0.605485603995113));
#14990=CARTESIAN_POINT('Ctrl Pts',(1.09999999916631,-1.24553911263843,0.605485603997431));
#14991=CARTESIAN_POINT('Ctrl Pts',(1.10000000220634,-1.24510362317222,0.61339691285734));
#14992=CARTESIAN_POINT('Ctrl Pts',(1.10000177015643,-1.24370036622144,0.621215229994996));
#14993=CARTESIAN_POINT('Ctrl Pts',(1.10000252895322,-1.24141353486351,0.628780213666851));
#14994=CARTESIAN_POINT('Ctrl Pts',(1.10000294802756,-1.24015054543059,0.632958263090869));
#14995=CARTESIAN_POINT('Ctrl Pts',(1.10000312162076,-1.23861706177488,0.637059070655947));
#14996=CARTESIAN_POINT('Ctrl Pts',(1.10000299297862,-1.23682078380192,0.641053713130525));
#14997=CARTESIAN_POINT('Ctrl Pts',(1.10000275999609,-1.23356756237267,0.64828837095969));
#14998=CARTESIAN_POINT('Ctrl Pts',(1.10000138715103,-1.22949085733774,0.655096441442141));
#14999=CARTESIAN_POINT('Ctrl Pts',(1.10000084482056,-1.2246552743941,0.661315040399663));
#15000=CARTESIAN_POINT('Ctrl Pts',(1.10000074196669,-1.22373819809959,0.662494407966206));
#15001=CARTESIAN_POINT('Ctrl Pts',(1.1000006773267,-1.22279369438101,0.663652502541609));
#15002=CARTESIAN_POINT('Ctrl Pts',(1.10000067553493,-1.22182202641035,0.66478809188211));
#15003=CARTESIAN_POINT('Ctrl Pts',(1.10000067210542,-1.219962222636,0.666961646435043));
#15004=CARTESIAN_POINT('Ctrl Pts',(1.10000089707048,-1.21800293160495,0.669052796220007));
#15005=CARTESIAN_POINT('Ctrl Pts',(1.10000120920309,-1.21595100691259,0.671058078730413));
#15006=CARTESIAN_POINT('Ctrl Pts',(1.10000207391986,-1.21026645613745,0.676613414309409));
#15007=CARTESIAN_POINT('Ctrl Pts',(1.1000034579227,-1.20393786500476,0.681450029097565));
#15008=CARTESIAN_POINT('Ctrl Pts',(1.10000394126019,-1.19712964857754,0.685514663758263));
#15009=CARTESIAN_POINT('Ctrl Pts',(1.10000424974863,-1.19278432848208,0.688108902478585));
#15010=CARTESIAN_POINT('Ctrl Pts',(1.10000425197701,-1.18824265871575,0.690387991283085));
#15011=CARTESIAN_POINT('Ctrl Pts',(1.10000394032285,-1.18354156621637,0.692328715646671));
#15012=CARTESIAN_POINT('Ctrl Pts',(1.10000345443802,-1.17621232165581,0.695354404566264));
#15013=CARTESIAN_POINT('Ctrl Pts',(1.10000219938511,-1.16858027633095,0.697525330589554));
#15014=CARTESIAN_POINT('Ctrl Pts',(1.10000118192936,-1.16079305972554,0.698772417158578));
#15015=CARTESIAN_POINT('Ctrl Pts',(1.10000052251962,-1.15574619011492,0.699580649884844));
#15016=CARTESIAN_POINT('Ctrl Pts',(1.1,-1.15063354328712,0.7));
#15017=CARTESIAN_POINT('Ctrl Pts',(1.1,-1.14549341399196,0.7));
#15018=CARTESIAN_POINT('',(1.1,-1.27885335043294,0.));
#15019=CARTESIAN_POINT('Ctrl Pts',(1.1,-1.27885335043294,0.));
#15020=CARTESIAN_POINT('Ctrl Pts',(1.1,-1.27330503870861,0.100887457206881));
#15021=CARTESIAN_POINT('Ctrl Pts',(1.1,-1.26775537880223,0.201776123688554));
#15022=CARTESIAN_POINT('Ctrl Pts',(1.1,-1.25665069275548,0.403603798678134));
#15023=CARTESIAN_POINT('Ctrl Pts',(1.1,-1.25109552364596,0.504545380833391));
#15024=CARTESIAN_POINT('Ctrl Pts',(1.1,-1.24553911298206,0.605485603995113));
#15025=CARTESIAN_POINT('',(1.1,-1.34328341716202,0.));
#15026=CARTESIAN_POINT('Origin',(0.199725906950915,-1.4,-0.0104671912485888));
#15027=CARTESIAN_POINT('',(0.200274469199584,1.12301388185427,1.38777878078145E-17));
#15028=CARTESIAN_POINT('',(0.200274469199585,-0.7,0.));
#15029=CARTESIAN_POINT('',(0.231993417893744,1.09142177001972,0.605233595624295));
#15030=CARTESIAN_POINT('Ctrl Pts',(0.200274469199584,1.12301388185427,-2.97071395261028E-17));
#15031=CARTESIAN_POINT('Ctrl Pts',(0.210847451470635,1.11248294808,0.201744519910852));
#15032=CARTESIAN_POINT('Ctrl Pts',(0.22142043436526,1.101952242875,0.403489051720196));
#15033=CARTESIAN_POINT('Ctrl Pts',(0.231993417893744,1.09142177001972,0.605233595624295));
#15034=CARTESIAN_POINT('',(0.231993417893744,-1.09142177001972,0.605233595624295));
#15035=CARTESIAN_POINT('',(0.231993417893744,-0.7,0.605233595624295));
#15036=CARTESIAN_POINT('',(0.200274469199584,-1.12301388185427,-1.38777878078145E-17));
#15037=CARTESIAN_POINT('Ctrl Pts',(0.231993417893744,-1.09142177001972,
0.605233595624295));
#15038=CARTESIAN_POINT('Ctrl Pts',(0.22142043436526,-1.101952242875,0.403489051720196));
#15039=CARTESIAN_POINT('Ctrl Pts',(0.210847451470635,-1.11248294808,0.201744519910852));
#15040=CARTESIAN_POINT('Ctrl Pts',(0.200274469199584,-1.12301388185427,
-4.90059381963448E-17));
#15041=CARTESIAN_POINT('',(0.200274469199585,-0.7,0.));
#15042=CARTESIAN_POINT('Origin',(5.4,-1.11022302462516E-16,0.));
#15043=CARTESIAN_POINT('Ctrl Pts',(7.29999999999999,-1.35236351479115,1.04083408558608E-17));
#15044=CARTESIAN_POINT('Ctrl Pts',(8.20044803681595,-1.32637404707459,3.18306896032855E-8));
#15045=CARTESIAN_POINT('Ctrl Pts',(9.10060048441536,-1.28803709316692,1.03188250195688E-8));
#15046=CARTESIAN_POINT('Ctrl Pts',(10.0000000000405,-1.24211782537639,-8.23328475353175E-12));
#15047=CARTESIAN_POINT('Ctrl Pts',(10.0000000000405,1.24211782537639,-8.23320567538283E-12));
#15048=CARTESIAN_POINT('Ctrl Pts',(9.1006004808701,1.28803709334794,1.03184817085883E-8));
#15049=CARTESIAN_POINT('Ctrl Pts',(8.20044803144508,1.32637404722969,3.18291413954212E-8));
#15050=CARTESIAN_POINT('Ctrl Pts',(7.3,1.35236351479115,4.75121773919879E-17));
#15051=CARTESIAN_POINT('',(7.1,1.35793097395724,0.));
#15052=CARTESIAN_POINT('',(7.1,1.42555555555556,0.));
#15053=CARTESIAN_POINT('Ctrl Pts',(7.1000000000396,1.35793097389613,-4.88924676637329E-12));
#15054=CARTESIAN_POINT('Ctrl Pts',(6.53177385320612,1.37316067096195,3.71763852401782E-9));
#15055=CARTESIAN_POINT('Ctrl Pts',(5.96344379069665,1.38333257666104,-3.82408184804385E-8));
#15056=CARTESIAN_POINT('Ctrl Pts',(5.39512359652123,1.38725406840392,-3.97623797275691E-8));
#15057=CARTESIAN_POINT('Ctrl Pts',(4.82973248928002,1.39115534902226,-4.12760989429076E-8));
#15058=CARTESIAN_POINT('Ctrl Pts',(4.26470859812609,1.38886839226708,1.63957607983357E-8));
#15059=CARTESIAN_POINT('Ctrl Pts',(3.70000000036239,1.37924639538501,-6.25376529969227E-12));
#15060=CARTESIAN_POINT('',(3.5,1.37552980833516,0.));
#15061=CARTESIAN_POINT('',(3.5,1.44777777777778,0.));
#15062=CARTESIAN_POINT('Ctrl Pts',(3.50000000097466,1.37552980835479,1.06251812903579E-15));
#15063=CARTESIAN_POINT('Ctrl Pts',(2.69943075695685,1.35940904975719,2.35366119539541E-7));
#15064=CARTESIAN_POINT('Ctrl Pts',(1.89948254587541,1.32827224396921,2.51300192353997E-7));
#15065=CARTESIAN_POINT('Ctrl Pts',(1.10000000028363,1.27885335028943,-5.13283415455519E-11));
#15066=CARTESIAN_POINT('',(0.9,1.266106713614,0.));
#15067=CARTESIAN_POINT('',(0.9,1.34328341716202,0.));
#15068=CARTESIAN_POINT('',(0.292382661757373,1.22257596919059,0.));
#15069=CARTESIAN_POINT('Ctrl Pts',(0.9,1.266106713614,1.20346441145891E-16));
#15070=CARTESIAN_POINT('Ctrl Pts',(0.697432754539207,1.25280566772398,-2.10387859372414E-8));
#15071=CARTESIAN_POINT('Ctrl Pts',(0.494894520889663,1.23831317328004,3.6654767345328E-12));
#15072=CARTESIAN_POINT('Ctrl Pts',(0.292382661757371,1.22257596919059,2.98331735103528E-16));
#15073=CARTESIAN_POINT('Ctrl Pts',(0.292382661757373,1.22257596919059,2.94902990916057E-17));
#15074=CARTESIAN_POINT('Ctrl Pts',(0.284469747869226,1.22196105627757,-8.65621238729993E-13));
#15075=CARTESIAN_POINT('Ctrl Pts',(0.276673396002317,1.22038240716686,-1.19564355630166E-6));
#15076=CARTESIAN_POINT('Ctrl Pts',(0.269153172408756,1.21792571627104,-1.29137975931779E-6));
#15077=CARTESIAN_POINT('Ctrl Pts',(0.264330998492885,1.21635041859408,-1.35276844214688E-6));
#15078=CARTESIAN_POINT('Ctrl Pts',(0.259622238853914,1.21441292414196,-1.0165784587106E-6));
#15079=CARTESIAN_POINT('Ctrl Pts',(0.255072584042237,1.21212521597766,-4.21167369976509E-7));
#15080=CARTESIAN_POINT('Ctrl Pts',(0.247984787860257,1.20856125126747,5.06409032217246E-7));
#15081=CARTESIAN_POINT('Ctrl Pts',(0.241364979299678,1.20419126978451,2.25366520907849E-6));
#15082=CARTESIAN_POINT('Ctrl Pts',(0.235375785094684,1.19908071490398,1.28723124315333E-6));
#15083=CARTESIAN_POINT('Ctrl Pts',(0.235058634311792,1.19881009144014,1.23605486142058E-6));
#15084=CARTESIAN_POINT('Ctrl Pts',(0.234743258170683,1.19853738091759,1.17639378419006E-6));
#15085=CARTESIAN_POINT('Ctrl Pts',(0.234429683218046,1.19826258967301,1.10742116603597E-6));
#15086=CARTESIAN_POINT('Ctrl Pts',(0.23095881299434,1.19522100506769,3.4398325561458E-7));
#15087=CARTESIAN_POINT('Ctrl Pts',(0.227708211416394,1.19192479473749,-1.52348441667556E-6));
#15088=CARTESIAN_POINT('Ctrl Pts',(0.224692430858345,1.18840300965977,-3.42436181452249E-6));
#15089=CARTESIAN_POINT('Ctrl Pts',(0.219522873151367,1.18236607466387,-6.68278702580898E-6));
#15090=CARTESIAN_POINT('Ctrl Pts',(0.21509942609515,1.17573654654733,-9.78259773483875E-6));
#15091=CARTESIAN_POINT('Ctrl Pts',(0.211478909386775,1.16867548752938,-1.04320859863301E-5));
#15092=CARTESIAN_POINT('Ctrl Pts',(0.20968494559888,1.16517673715679,-1.075390701291E-5));
#15093=CARTESIAN_POINT('Ctrl Pts',(0.208088728862602,1.16157146972622,-1.05358292927083E-5));
#15094=CARTESIAN_POINT('Ctrl Pts',(0.206701335101202,1.15787708229469,-9.83193564179307E-6));
#15095=CARTESIAN_POINT('Ctrl Pts',(0.203919119965097,1.15046852899383,-8.42037994342582E-6));
#15096=CARTESIAN_POINT('Ctrl Pts',(0.202003457218558,1.1427818296106,-4.88542801801716E-6));
#15097=CARTESIAN_POINT('Ctrl Pts',(0.201024541128784,1.13496408391561,-2.30807221316776E-6));
#15098=CARTESIAN_POINT('Ctrl Pts',(0.200529226009753,1.13100843574523,-1.00397341389412E-6));
#15099=CARTESIAN_POINT('Ctrl Pts',(0.200274469344113,1.12701892049093,-1.14168925800036E-11));
#15100=CARTESIAN_POINT('Ctrl Pts',(0.200274469199584,1.12301388185427,-1.43114686768087E-17));
#15101=CARTESIAN_POINT('',(-1.73234772679968E-18,1.12356026268968,4.53319947845445E-20));
#15102=CARTESIAN_POINT('',(0.,-1.4,0.));
#15103=CARTESIAN_POINT('',(0.276326924564679,1.42224670711126,-2.77555756156289E-17));
#15104=CARTESIAN_POINT('Ctrl Pts',(0.276326924564681,1.42224670711126,-1.50920942409982E-16));
#15105=CARTESIAN_POINT('Ctrl Pts',(0.258529852003869,1.4208638358667,-3.32972379743633E-13));
#15106=CARTESIAN_POINT('Ctrl Pts',(0.240927013527826,1.41785398988725,-1.99727536601662E-6));
#15107=CARTESIAN_POINT('Ctrl Pts',(0.223720619657732,1.41333325652174,-2.71091968639774E-6));
#15108=CARTESIAN_POINT('Ctrl Pts',(0.206313289378911,1.40875972999491,-3.432897951005E-6));
#15109=CARTESIAN_POINT('Ctrl Pts',(0.18931019325249,1.40263932318529,-2.78724979559428E-6));
#15110=CARTESIAN_POINT('Ctrl Pts',(0.172932985028856,1.39504220432096,-6.31841720307455E-7));
#15111=CARTESIAN_POINT('Ctrl Pts',(0.170060146426803,1.39370954151055,-2.53746782677961E-7));
#15112=CARTESIAN_POINT('Ctrl Pts',(0.167206630967902,1.39233132643846,1.61597591574489E-7));
#15113=CARTESIAN_POINT('Ctrl Pts',(0.164373729059928,1.39090779908693,6.02790108062464E-7));
#15114=CARTESIAN_POINT('Ctrl Pts',(0.148213121449433,1.38278712717586,3.11962244863226E-6));
#15115=CARTESIAN_POINT('Ctrl Pts',(0.132864864406694,1.37326763401578,6.8005293729143E-6));
#15116=CARTESIAN_POINT('Ctrl Pts',(0.118540368157823,1.36244192017091,7.47011412280372E-6));
#15117=CARTESIAN_POINT('Ctrl Pts',(0.1130124780146,1.35826422653222,7.72851001154276E-6));
#15118=CARTESIAN_POINT('Ctrl Pts',(0.107637267132642,1.35389150739715,7.50091387420595E-6));
#15119=CARTESIAN_POINT('Ctrl Pts',(0.102427993107927,1.34932731552598,6.39696583889361E-6));
#15120=CARTESIAN_POINT('Ctrl Pts',(0.0920147884934566,1.34020361352282,
4.19020214765608E-6));
#15121=CARTESIAN_POINT('Ctrl Pts',(0.082263696775192,1.33031540618347,-1.43705507633734E-6));
#15122=CARTESIAN_POINT('Ctrl Pts',(0.0732179607829324,1.31975004019149,
-7.24116446069057E-6));
#15123=CARTESIAN_POINT('Ctrl Pts',(0.0614369648181435,1.30598990677343,
-1.48003270644599E-5));
#15124=CARTESIAN_POINT('Ctrl Pts',(0.0509520748529884,1.29120077200215,
-2.24515165560165E-5));
#15125=CARTESIAN_POINT('Ctrl Pts',(0.0418305631051555,1.27560026299671,
-2.64881615939377E-5));
#15126=CARTESIAN_POINT('Ctrl Pts',(0.0329966685655992,1.26049166530727,
-3.03975241584371E-5));
#15127=CARTESIAN_POINT('Ctrl Pts',(0.0254411283904758,1.24462062939249,
-3.09701348507133E-5));
#15128=CARTESIAN_POINT('Ctrl Pts',(0.0192647836588538,1.2281607987719,-2.81763116144976E-5));
#15129=CARTESIAN_POINT('Ctrl Pts',(0.0129258683931997,1.2112677210496,-2.53089508159798E-5));
#15130=CARTESIAN_POINT('Ctrl Pts',(0.00809110271874438,1.19389182855556,
-1.89493195503086E-5));
#15131=CARTESIAN_POINT('Ctrl Pts',(0.00484442764459327,1.17622983835018,
-1.25518552566888E-5));
#15132=CARTESIAN_POINT('Ctrl Pts',(0.00165723550742335,1.1588914367474,
-6.27160009448058E-6));
#15133=CARTESIAN_POINT('Ctrl Pts',(1.90718451428807E-9,1.14127598190669,
-1.51296892603399E-10));
#15134=CARTESIAN_POINT('Ctrl Pts',(2.41777084464267E-17,1.12356026268968,
-3.46944695195361E-18));
#15135=CARTESIAN_POINT('',(10.5166159648474,1.4155315881283,0.));
#15136=CARTESIAN_POINT('Ctrl Pts',(0.276326924564679,1.42224670711126,0.));
#15137=CARTESIAN_POINT('Ctrl Pts',(3.68975660465893,1.68747752195839,0.));
#15138=CARTESIAN_POINT('Ctrl Pts',(7.10318628475318,1.599994843061,0.));
#15139=CARTESIAN_POINT('Ctrl Pts',(10.5166159648474,1.4155315881283,0.));
#15140=CARTESIAN_POINT('',(10.8,1.11638029377732,-5.56631991785941E-17));
#15141=CARTESIAN_POINT('Ctrl Pts',(10.8,1.11638029377732,2.32452945780892E-16));
#15142=CARTESIAN_POINT('Ctrl Pts',(10.7999999994302,1.13421844616111,-9.29296349749781E-12));
#15143=CARTESIAN_POINT('Ctrl Pts',(10.7983603663884,1.15198349698667,-2.38856955364628E-6));
#15144=CARTESIAN_POINT('Ctrl Pts',(10.7951843826221,1.16946861094468,-3.77014304120448E-6));
#15145=CARTESIAN_POINT('Ctrl Pts',(10.7919669771209,1.18718176881198,-5.16973525142236E-6));
#15146=CARTESIAN_POINT('Ctrl Pts',(10.7871724978816,1.20460918321158,-5.4755482503851E-6));
#15147=CARTESIAN_POINT('Ctrl Pts',(10.7808573412527,1.22152732075962,-4.27334038376583E-6));
#15148=CARTESIAN_POINT('Ctrl Pts',(10.7797421066656,1.22451500471617,-4.06103467663179E-6));
#15149=CARTESIAN_POINT('Ctrl Pts',(10.7785793293545,1.22748675045939,-3.81081650224554E-6));
#15150=CARTESIAN_POINT('Ctrl Pts',(10.7773691713543,1.23044124224994,-3.53261416912234E-6));
#15151=CARTESIAN_POINT('Ctrl Pts',(10.7705159051166,1.24717287467681,-1.95712183132163E-6));
#15152=CARTESIAN_POINT('Ctrl Pts',(10.7622076549587,1.26320448426569,8.50150473021234E-7));
#15153=CARTESIAN_POINT('Ctrl Pts',(10.7525236566209,1.27832128496499,1.09915986206012E-6));
#15154=CARTESIAN_POINT('Ctrl Pts',(10.7482509716548,1.28499098118248,1.20902550183604E-6));
#15155=CARTESIAN_POINT('Ctrl Pts',(10.7437098328292,1.29148238441373,7.76315258636623E-7));
#15156=CARTESIAN_POINT('Ctrl Pts',(10.7389041877712,1.29777551763099,-7.54184826032082E-7));
#15157=CARTESIAN_POINT('Ctrl Pts',(10.7310976851069,1.30799836193882,-3.24039694621926E-6));
#15158=CARTESIAN_POINT('Ctrl Pts',(10.7225935645301,1.31769858917671,-8.57388820182801E-6));
#15159=CARTESIAN_POINT('Ctrl Pts',(10.7134588931078,1.3268364513864,-1.41086939541967E-5));
#15160=CARTESIAN_POINT('Ctrl Pts',(10.7004433550849,1.33985653580309,-2.19949628070403E-5));
#15161=CARTESIAN_POINT('Ctrl Pts',(10.6862650266646,1.35162127070648,-3.0022236679635E-5));
#15162=CARTESIAN_POINT('Ctrl Pts',(10.6711476119081,1.36204513612776,-3.40981369893719E-5));
#15163=CARTESIAN_POINT('Ctrl Pts',(10.6560301971515,1.37246900154903,-3.81740372991087E-5));
#15164=CARTESIAN_POINT('Ctrl Pts',(10.6399721826852,1.38155285075117,-3.83332859284948E-5));
#15165=CARTESIAN_POINT('Ctrl Pts',(10.6231652498763,1.38916602817047,-3.45204725343976E-5));
#15166=CARTESIAN_POINT('Ctrl Pts',(10.6063487480974,1.39678354012646,-3.07054883279539E-5));
#15167=CARTESIAN_POINT('Ctrl Pts',(10.5889271210941,1.40286310406803,-2.29928881382306E-5));
#15168=CARTESIAN_POINT('Ctrl Pts',(10.5711041279812,1.40730078588308,-1.53078138731408E-5));
#15169=CARTESIAN_POINT('Ctrl Pts',(10.5532811348684,1.41173846769814,-7.6227396080509E-6));
#15170=CARTESIAN_POINT('Ctrl Pts',(10.5350552605908,1.41453511891929,-9.16729947674095E-11));
#15171=CARTESIAN_POINT('Ctrl Pts',(10.5166159648474,1.4155315881283,2.48932818802672E-16));
#15172=CARTESIAN_POINT('',(10.8,-1.11638029377732,-1.39157997946485E-17));
#15173=CARTESIAN_POINT('',(10.8,1.4,0.));
#15174=CARTESIAN_POINT('',(10.5166159648474,-1.4155315881283,2.77555756156289E-17));
#15175=CARTESIAN_POINT('Ctrl Pts',(10.5166159648474,-1.4155315881283,-1.94289029309402E-16));
#15176=CARTESIAN_POINT('Ctrl Pts',(10.5344251606169,-1.41456917089032,1.72780596414851E-12));
#15177=CARTESIAN_POINT('Ctrl Pts',(10.5520727686739,-1.41197333457428,-2.53403886306205E-6));
#15178=CARTESIAN_POINT('Ctrl Pts',(10.5693578805681,-1.40785843881911,-4.04156906196095E-6));
#15179=CARTESIAN_POINT('Ctrl Pts',(10.5868701251756,-1.40368947182374,-5.56890876087065E-6));
#15180=CARTESIAN_POINT('Ctrl Pts',(10.604011804524,-1.39796079212135,-5.98742339745246E-6));
#15181=CARTESIAN_POINT('Ctrl Pts',(10.6205627760847,-1.39074087128671,-4.81856832951796E-6));
#15182=CARTESIAN_POINT('Ctrl Pts',(10.6234754753687,-1.38947028374636,-4.61286902618664E-6));
#15183=CARTESIAN_POINT('Ctrl Pts',(10.6263698187278,-1.38815339768352,-4.36721670635639E-6));
#15184=CARTESIAN_POINT('Ctrl Pts',(10.629244514885,-1.38679044403738,-4.09122931699412E-6));
#15185=CARTESIAN_POINT('Ctrl Pts',(10.6455827855986,-1.37904412775797,-2.5226612199239E-6));
#15186=CARTESIAN_POINT('Ctrl Pts',(10.6611432679573,-1.36988219838444,3.58605122725343E-7));
#15187=CARTESIAN_POINT('Ctrl Pts',(10.6757157985124,-1.35939560704671,7.40589063327193E-7));
#15188=CARTESIAN_POINT('Ctrl Pts',(10.6821516119741,-1.35476430808026,9.09288478831296E-7));
#15189=CARTESIAN_POINT('Ctrl Pts',(10.6883944859408,-1.34987400891586,5.44816430868337E-7));
#15190=CARTESIAN_POINT('Ctrl Pts',(10.6944246343503,-1.34472976213865,-9.14752338109426E-7));
#15191=CARTESIAN_POINT('Ctrl Pts',(10.7041966733629,-1.33639335368171,-3.28002794718031E-6));
#15192=CARTESIAN_POINT('Ctrl Pts',(10.7134106653983,-1.3273903805878,-8.47259327327479E-6));
#15193=CARTESIAN_POINT('Ctrl Pts',(10.7220307555455,-1.31778973409553,-1.38734771921913E-5));
#15194=CARTESIAN_POINT('Ctrl Pts',(10.7343338492722,-1.3040871333553,-2.15819326638919E-5));
#15195=CARTESIAN_POINT('Ctrl Pts',(10.7453199276401,-1.28929041974124,-2.94555326738194E-5));
#15196=CARTESIAN_POINT('Ctrl Pts',(10.7549158277293,-1.27362793268665,-3.3443536645081E-5));
#15197=CARTESIAN_POINT('Ctrl Pts',(10.7645117278185,-1.25796544563206,-3.74315406163426E-5));
#15198=CARTESIAN_POINT('Ctrl Pts',(10.7727182208071,-1.24143562566754,-3.75750290962259E-5));
#15199=CARTESIAN_POINT('Ctrl Pts',(10.7794153247677,-1.22423716044977,-3.38265125308188E-5));
#15200=CARTESIAN_POINT('Ctrl Pts',(10.7861166764432,-1.20702778690835,-3.00756184258222E-5));
#15201=CARTESIAN_POINT('Ctrl Pts',(10.7912490477072,-1.18929683429644,-2.25107044755726E-5));
#15202=CARTESIAN_POINT('Ctrl Pts',(10.7947196858669,-1.17125359626911,-1.49815203503087E-5));
#15203=CARTESIAN_POINT('Ctrl Pts',(10.7981903240266,-1.15321035824179,-7.45233622504479E-6));
#15204=CARTESIAN_POINT('Ctrl Pts',(10.7999999985278,-1.13485327409571,-1.17780195603766E-10));
#15205=CARTESIAN_POINT('Ctrl Pts',(10.8,-1.11638029377732,-1.38777878078145E-17));
#15206=CARTESIAN_POINT('',(0.276326924564679,-1.42224670711126,-5.55111512312578E-17));
#15207=CARTESIAN_POINT('Ctrl Pts',(10.5166159648474,-1.4155315881283,0.));
#15208=CARTESIAN_POINT('Ctrl Pts',(7.10318628475318,-1.599994843061,0.));
#15209=CARTESIAN_POINT('Ctrl Pts',(3.68975660465893,-1.68747752195839,0.));
#15210=CARTESIAN_POINT('Ctrl Pts',(0.276326924564679,-1.42224670711126,
0.));
#15211=CARTESIAN_POINT('',(-7.25311916552711E-19,-1.12356026268968,1.39157997946485E-17));
#15212=CARTESIAN_POINT('Ctrl Pts',(1.80411241501588E-16,-1.12356026268968,
-1.53523027623947E-16));
#15213=CARTESIAN_POINT('Ctrl Pts',(7.41078168374529E-10,-1.14141522098415,
-1.3067981184062E-11));
#15214=CARTESIAN_POINT('Ctrl Pts',(0.00163694718329378,-1.15920272117896,
-1.78823819589733E-6));
#15215=CARTESIAN_POINT('Ctrl Pts',(0.00481087395297265,-1.17671209893291,
-2.3181425555783E-6));
#15216=CARTESIAN_POINT('Ctrl Pts',(0.00802138847203439,-1.19442331774104,
-2.85415543927884E-6));
#15217=CARTESIAN_POINT('Ctrl Pts',(0.0128049030182357,-1.21185152247087,
-2.04128886843626E-6));
#15218=CARTESIAN_POINT('Ctrl Pts',(0.0191087770915565,-1.22877027194193,
1.71240493184593E-7));
#15219=CARTESIAN_POINT('Ctrl Pts',(0.0202201941454154,-1.23175316571065,
5.613248819379E-7));
#15220=CARTESIAN_POINT('Ctrl Pts',(0.0213789882593307,-1.23472016785247,
9.85829603970989E-7));
#15221=CARTESIAN_POINT('Ctrl Pts',(0.0225850188675993,-1.23766995297306,
1.43287414332239E-6));
#15222=CARTESIAN_POINT('Ctrl Pts',(0.0294291562303479,-1.25440977235863,
3.96981990042924E-6));
#15223=CARTESIAN_POINT('Ctrl Pts',(0.0377300686697735,-1.27044838970616,
7.55798501181421E-6));
#15224=CARTESIAN_POINT('Ctrl Pts',(0.0474121614036163,-1.28556782977674,
8.05058320302158E-6));
#15225=CARTESIAN_POINT('Ctrl Pts',(0.0511425121829324,-1.29139310088294,
8.24037316857697E-6));
#15226=CARTESIAN_POINT('Ctrl Pts',(0.0550784035723718,-1.29708174651376,
7.93435480917585E-6));
#15227=CARTESIAN_POINT('Ctrl Pts',(0.0592173503759339,-1.30262033374061,
6.74858081742264E-6));
#15228=CARTESIAN_POINT('Ctrl Pts',(0.0675201807396794,-1.31373087764993,
4.36988865960166E-6));
#15229=CARTESIAN_POINT('Ctrl Pts',(0.0766394565597649,-1.32423847988766,
-1.46587651676554E-6));
#15230=CARTESIAN_POINT('Ctrl Pts',(0.0864911062490747,-1.33409287340636,
-7.46705500292641E-6));
#15231=CARTESIAN_POINT('Ctrl Pts',(0.0992988409846585,-1.34690417528452,
-1.52689465211603E-5));
#15232=CARTESIAN_POINT('Ctrl Pts',(0.113232871116931,-1.35850278376499,
-2.31308069859054E-5));
#15233=CARTESIAN_POINT('Ctrl Pts',(0.128081622025101,-1.36880445085772,
-2.72849174168177E-5));
#15234=CARTESIAN_POINT('Ctrl Pts',(0.142447925282442,-1.37877140864598,
-3.13040575171566E-5));
#15235=CARTESIAN_POINT('Ctrl Pts',(0.157671864768995,-1.38752483454192,
-3.1899138628041E-5));
#15236=CARTESIAN_POINT('Ctrl Pts',(0.173588691395025,-1.39495074934422,
-2.90326641197332E-5));
#15237=CARTESIAN_POINT('Ctrl Pts',(0.189936400238013,-1.40257769006131,
-2.60885916756054E-5));
#15238=CARTESIAN_POINT('Ctrl Pts',(0.206881864105471,-1.40874232120582,
-1.95409011442111E-5));
#15239=CARTESIAN_POINT('Ctrl Pts',(0.22423558959196,-1.41334558507228,-1.29462590315495E-5));
#15240=CARTESIAN_POINT('Ctrl Pts',(0.241260467995769,-1.4178616186841,-6.47658310103417E-6));
#15241=CARTESIAN_POINT('Ctrl Pts',(0.258679581942429,-1.42087546890512,
-1.12101563992788E-10));
#15242=CARTESIAN_POINT('Ctrl Pts',(0.27632692456468,-1.42224670711126,1.05818132034585E-16));
#15243=CARTESIAN_POINT('',(0.,-1.4,0.));
#15244=CARTESIAN_POINT('',(0.292382661757373,-1.22257596919059,0.));
#15245=CARTESIAN_POINT('Ctrl Pts',(0.200274469199584,-1.12301388185427,
-2.68882138776405E-17));
#15246=CARTESIAN_POINT('Ctrl Pts',(0.200274469314753,-1.13095194822878,
-2.85686379674833E-12));
#15247=CARTESIAN_POINT('Ctrl Pts',(0.201244085522878,-1.13884856843413,
-1.08105759021766E-6));
#15248=CARTESIAN_POINT('Ctrl Pts',(0.203110344361254,-1.14653799330522,
-1.10782444979703E-6));
#15249=CARTESIAN_POINT('Ctrl Pts',(0.204308287281872,-1.15147379958167,
-1.12500597321754E-6));
#15250=CARTESIAN_POINT('Ctrl Pts',(0.205876831658669,-1.15632444796435,
-7.573778542164E-7));
#15251=CARTESIAN_POINT('Ctrl Pts',(0.207807574899602,-1.16104329283393,
-1.57887042599725E-7));
#15252=CARTESIAN_POINT('Ctrl Pts',(0.21096922807971,-1.1687705506961,8.23798139982571E-7));
#15253=CARTESIAN_POINT('Ctrl Pts',(0.215060220496011,-1.17605061753432,
2.67511715935828E-6));
#15254=CARTESIAN_POINT('Ctrl Pts',(0.220020901709485,-1.18268777995331,
1.20301732358232E-6));
#15255=CARTESIAN_POINT('Ctrl Pts',(0.222788929945646,-1.18639127392786,
3.81595076007225E-7));
#15256=CARTESIAN_POINT('Ctrl Pts',(0.225828882930032,-1.18989419630164,
-1.55522758636672E-6));
#15257=CARTESIAN_POINT('Ctrl Pts',(0.229112809647272,-1.19317965616817,
-3.52099818518546E-6));
#15258=CARTESIAN_POINT('Ctrl Pts',(0.234731790749985,-1.1988012605745,-6.88454091865859E-6));
#15259=CARTESIAN_POINT('Ctrl Pts',(0.240999377733319,-1.20372479786492,
-1.00686973618824E-5));
#15260=CARTESIAN_POINT('Ctrl Pts',(0.247759525934523,-1.2078808899968,-1.07387199666626E-5));
#15261=CARTESIAN_POINT('Ctrl Pts',(0.251104201987095,-1.20993717358883,
-1.10702228411842E-5));
#15262=CARTESIAN_POINT('Ctrl Pts',(0.254570062984725,-1.21180502729412,
-1.08478245319173E-5));
#15263=CARTESIAN_POINT('Ctrl Pts',(0.258140701417296,-1.21347208138814,
-1.01264154182862E-5));
#15264=CARTESIAN_POINT('Ctrl Pts',(0.265309933881728,-1.21681924144269,
-8.67794906268977E-6));
#15265=CARTESIAN_POINT('Ctrl Pts',(0.27282354441991,-1.21932394229889,-5.03816435877804E-6));
#15266=CARTESIAN_POINT('Ctrl Pts',(0.280540402387729,-1.22090470300999,
-2.38011023443526E-6));
#15267=CARTESIAN_POINT('Ctrl Pts',(0.284441227387562,-1.22170376798259,
-1.03647996128718E-6));
#15268=CARTESIAN_POINT('Ctrl Pts',(0.288394358015454,-1.22226603782358,
-8.41267709508591E-12));
#15269=CARTESIAN_POINT('Ctrl Pts',(0.292382661757373,-1.22257596919059,
3.10081821330854E-17));
#15270=CARTESIAN_POINT('',(0.9,-1.266106713614,0.));
#15271=CARTESIAN_POINT('Ctrl Pts',(0.29238266175737,-1.22257596919059,3.4274341177698E-16));
#15272=CARTESIAN_POINT('Ctrl Pts',(0.494894519961671,-1.23831317320793,
3.6654050078524E-12));
#15273=CARTESIAN_POINT('Ctrl Pts',(0.697432753591781,-1.25280566766171,
-2.10377631034678E-8));
#15274=CARTESIAN_POINT('Ctrl Pts',(0.900000000000002,-1.266106713614,4.80511808774455E-17));
#15275=CARTESIAN_POINT('',(0.9,1.34328341716202,0.));
#15276=CARTESIAN_POINT('',(3.5,-1.37552980833516,0.));
#15277=CARTESIAN_POINT('Ctrl Pts',(1.10000000028363,-1.27885335028943,-5.13283219638443E-11));
#15278=CARTESIAN_POINT('Ctrl Pts',(1.8994825293422,-1.32827224294784,2.51289069808066E-7));
#15279=CARTESIAN_POINT('Ctrl Pts',(2.69943073922525,-1.35940904940056,2.35357980118634E-7));
#15280=CARTESIAN_POINT('Ctrl Pts',(3.50000000097418,-1.37552980835478,8.59034485311056E-16));
#15281=CARTESIAN_POINT('',(3.5,1.44777777777778,0.));
#15282=CARTESIAN_POINT('',(7.1,-1.35793097395724,0.));
#15283=CARTESIAN_POINT('Ctrl Pts',(3.700000000362,-1.379246395385,-6.25385501848083E-12));
#15284=CARTESIAN_POINT('Ctrl Pts',(4.26467016042339,-1.38886773733237,1.63880713394601E-8));
#15285=CARTESIAN_POINT('Ctrl Pts',(4.82965558050887,-1.39115503781354,-4.12727732537403E-8));
#15286=CARTESIAN_POINT('Ctrl Pts',(5.39500817395676,-1.38725486475042,-3.97626883737645E-8));
#15287=CARTESIAN_POINT('Ctrl Pts',(5.96336684492344,-1.38333395379258,-3.82445741104923E-8));
#15288=CARTESIAN_POINT('Ctrl Pts',(6.53173538886785,-1.37316170188981,3.71969681223073E-9));
#15289=CARTESIAN_POINT('Ctrl Pts',(7.1000000000396,-1.35793097389613,-4.88946831112289E-12));
#15290=CARTESIAN_POINT('',(7.1,1.42555555555556,0.));
#15291=CARTESIAN_POINT('',(10.2,-1.23178301601145,0.));
#15292=CARTESIAN_POINT('',(10.5052647440597,-1.21555035534119,0.));
#15293=CARTESIAN_POINT('Ctrl Pts',(10.2,-1.23178301601145,-4.56855690431079E-17));
#15294=CARTESIAN_POINT('Ctrl Pts',(10.3017652114452,-1.22646242153193,-6.28718440835499E-11));
#15295=CARTESIAN_POINT('Ctrl Pts',(10.4035203469111,-1.22104923788321,1.43982679105611E-13));
#15296=CARTESIAN_POINT('Ctrl Pts',(10.5052647440597,-1.21555035534119,6.44897004721534E-17));
#15297=CARTESIAN_POINT('',(10.5997255308004,-1.11583328740478,1.38777878078145E-17));
#15298=CARTESIAN_POINT('Ctrl Pts',(10.5052647440597,-1.21555035534119,-1.86482773667507E-17));
#15299=CARTESIAN_POINT('Ctrl Pts',(10.5131888530666,-1.21512208850275,-5.60416335832109E-13));
#15300=CARTESIAN_POINT('Ctrl Pts',(10.5210180054001,-1.21372544600509,-1.35972994235015E-6));
#15301=CARTESIAN_POINT('Ctrl Pts',(10.5285917824072,-1.2114444991589,-1.66070161277884E-6));
#15302=CARTESIAN_POINT('Ctrl Pts',(10.5334522234388,-1.20998071066451,-1.8538489757029E-6));
#15303=CARTESIAN_POINT('Ctrl Pts',(10.538207639053,-1.20815156029678,-1.66445033219183E-6));
#15304=CARTESIAN_POINT('Ctrl Pts',(10.542812250732,-1.20596855068549,-1.19054254011085E-6));
#15305=CARTESIAN_POINT('Ctrl Pts',(10.5499808226381,-1.20256998801374,-4.52751316616249E-7));
#15306=CARTESIAN_POINT('Ctrl Pts',(10.5567010840309,-1.19835579238971,1.16775294480959E-6));
#15307=CARTESIAN_POINT('Ctrl Pts',(10.5628099082467,-1.1933896765605,3.12218506849373E-7));
#15308=CARTESIAN_POINT('Ctrl Pts',(10.563392699667,-1.1929159013142,2.30599178383296E-7));
#15309=CARTESIAN_POINT('Ctrl Pts',(10.563969906567,-1.19243524850296,1.23643260424227E-7));
#15310=CARTESIAN_POINT('Ctrl Pts',(10.5645413730323,-1.19194775268147,-1.33988689923433E-8));
#15311=CARTESIAN_POINT('Ctrl Pts',(10.5677990734116,-1.18916873515523,-7.94620907596477E-7));
#15312=CARTESIAN_POINT('Ctrl Pts',(10.5708705204042,-1.18616755700159,-2.52696578471864E-6));
#15313=CARTESIAN_POINT('Ctrl Pts',(10.5737438185805,-1.18296717200411,-4.3349897000341E-6));
#15314=CARTESIAN_POINT('Ctrl Pts',(10.579054042416,-1.17705244973962,-7.67644996655303E-6));
#15315=CARTESIAN_POINT('Ctrl Pts',(10.5836289246435,-1.17052745137283,-1.0999028846932E-5));
#15316=CARTESIAN_POINT('Ctrl Pts',(10.5874112735695,-1.16355342251842,-1.18035167459916E-5));
#15317=CARTESIAN_POINT('Ctrl Pts',(10.5894705469099,-1.15975646143,-1.22415145393192E-5));
#15318=CARTESIAN_POINT('Ctrl Pts',(10.5912942421259,-1.15582570378367,-1.20038889321768E-5));
#15319=CARTESIAN_POINT('Ctrl Pts',(10.5928674986933,-1.15178403025788,-1.11465830745351E-5));
#15320=CARTESIAN_POINT('Ctrl Pts',(10.5957384082276,-1.14440870489779,-9.58215448007377E-6));
#15321=CARTESIAN_POINT('Ctrl Pts',(10.5977463817932,-1.13674651935037,-5.80208140981121E-6));
#15322=CARTESIAN_POINT('Ctrl Pts',(10.5988207707371,-1.12894377506163,-2.8960211281105E-6));
#15323=CARTESIAN_POINT('Ctrl Pts',(10.5994175893465,-1.12460938291963,-1.28171667533415E-6));
#15324=CARTESIAN_POINT('Ctrl Pts',(10.5997255306822,-1.12023121224821,-9.4020583932734E-12));
#15325=CARTESIAN_POINT('Ctrl Pts',(10.5997255308004,-1.11583328740478,-9.97465998686664E-18));
#15326=CARTESIAN_POINT('',(10.5997255308004,1.11583328740478,0.));
#15327=CARTESIAN_POINT('',(10.5997255308004,0.7,0.));
#15328=CARTESIAN_POINT('',(10.5052647440597,1.21555035534119,0.));
#15329=CARTESIAN_POINT('Ctrl Pts',(10.5997255308004,1.11583328740478,8.8037216405823E-17));
#15330=CARTESIAN_POINT('Ctrl Pts',(10.5997255307124,1.12376989384288,-2.22024716398596E-12));
#15331=CARTESIAN_POINT('Ctrl Pts',(10.5987536115518,1.13166401228391,-1.27532141444775E-6));
#15332=CARTESIAN_POINT('Ctrl Pts',(10.5968849989732,1.13935090273995,-1.5236651967046E-6));
#15333=CARTESIAN_POINT('Ctrl Pts',(10.5956849616024,1.14428748291596,-1.68315348385219E-6));
#15334=CARTESIAN_POINT('Ctrl Pts',(10.5941139374364,1.14913880701507,-1.46899737395989E-6));
#15335=CARTESIAN_POINT('Ctrl Pts',(10.5921809408638,1.1538584293407,-9.90118991603547E-7));
#15336=CARTESIAN_POINT('Ctrl Pts',(10.5891742477341,1.16119959911942,-2.45244239835432E-7));
#15337=CARTESIAN_POINT('Ctrl Pts',(10.5853292249979,1.16813727090899,1.33309554558619E-6));
#15338=CARTESIAN_POINT('Ctrl Pts',(10.5807005079991,1.17450509276749,4.08358240744415E-7));
#15339=CARTESIAN_POINT('Ctrl Pts',(10.5802604812716,1.17511044665166,3.20448539159982E-7));
#15340=CARTESIAN_POINT('Ctrl Pts',(10.5798133373602,1.17571063303672,2.07176952714776E-7));
#15341=CARTESIAN_POINT('Ctrl Pts',(10.5793591019426,1.17630549598644,6.38823567561716E-8));
#15342=CARTESIAN_POINT('Ctrl Pts',(10.5767566952267,1.17971358631841,-7.57081408668461E-7));
#15343=CARTESIAN_POINT('Ctrl Pts',(10.5739217504488,1.18294722379721,-2.53660858190298E-6));
#15344=CARTESIAN_POINT('Ctrl Pts',(10.570876618072,1.18599321478588,-4.38998728286835E-6));
#15345=CARTESIAN_POINT('Ctrl Pts',(10.5652565693637,1.19161484813492,-7.81055403847458E-6));
#15346=CARTESIAN_POINT('Ctrl Pts',(10.5589874561388,1.19653507038546,-1.11999964534866E-5));
#15347=CARTESIAN_POINT('Ctrl Pts',(10.5522271124844,1.20068789486255,-1.20263298844839E-5));
#15348=CARTESIAN_POINT('Ctrl Pts',(10.5485500617744,1.20294667739977,-1.24757848359648E-5));
#15349=CARTESIAN_POINT('Ctrl Pts',(10.5447269560479,1.20497781184918,-1.22374322375965E-5));
#15350=CARTESIAN_POINT('Ctrl Pts',(10.5407797717187,1.20676523914267,-1.13674773191707E-5));
#15351=CARTESIAN_POINT('Ctrl Pts',(10.5335711832013,1.210029547771,-9.77871264224002E-6));
#15352=CARTESIAN_POINT('Ctrl Pts',(10.5260296312848,1.21244761587922,-5.9245235663186E-6));
#15353=CARTESIAN_POINT('Ctrl Pts',(10.5182973307397,1.21394093281975,-2.95733858081469E-6));
#15354=CARTESIAN_POINT('Ctrl Pts',(10.514004731837,1.21476995008607,-1.31010113336685E-6));
#15355=CARTESIAN_POINT('Ctrl Pts',(10.5096528988527,1.21531319279956,-7.28166367327128E-12));
#15356=CARTESIAN_POINT('Ctrl Pts',(10.5052647440597,1.21555035534119,-3.31765864780564E-17));
#15357=CARTESIAN_POINT('',(10.2,1.23178301601145,0.));
#15358=CARTESIAN_POINT('Ctrl Pts',(10.5052647440597,1.21555035534119,1.20285454773689E-16));
#15359=CARTESIAN_POINT('Ctrl Pts',(10.4035203468995,1.22104923788384,1.44021921739714E-13));
#15360=CARTESIAN_POINT('Ctrl Pts',(10.3017652114309,1.22646242153268,-6.28696045710378E-11));
#15361=CARTESIAN_POINT('Ctrl Pts',(10.2,1.23178301601145,1.23125603768043E-16));
#15362=CARTESIAN_POINT('',(10.2,-1.30754691548544,0.));
#15363=CARTESIAN_POINT('Origin',(8.8,0.,0.));
#15364=CARTESIAN_POINT('',(8.4,-4.89858719658942E-17,0.));
#15365=CARTESIAN_POINT('Origin',(2.,0.,0.));
#15366=CARTESIAN_POINT('',(1.6,-4.89858719658941E-17,0.7));
#15367=CARTESIAN_POINT('Origin',(2.,0.,0.7));
#15368=CARTESIAN_POINT('',(1.6,-4.89858719658941E-17,0.));
#15369=CARTESIAN_POINT('Origin',(10.2,-1.30754691548544,0.));
#15370=CARTESIAN_POINT('',(10.1999999975107,-1.19856231453552,0.605472757505173));
#15371=CARTESIAN_POINT('Ctrl Pts',(10.2,-1.23178301601145,0.));
#15372=CARTESIAN_POINT('Ctrl Pts',(10.2,-1.22625045235593,0.100869147801815));
#15373=CARTESIAN_POINT('Ctrl Pts',(10.2,-1.22071692450357,0.201739022585575));
#15374=CARTESIAN_POINT('Ctrl Pts',(10.2,-1.2096433936729,0.403562754186249));
#15375=CARTESIAN_POINT('Ctrl Pts',(10.1999999975107,-1.20410330368611,0.50451817268257));
#15376=CARTESIAN_POINT('Ctrl Pts',(10.1999999975107,-1.19856231453552,0.605472757505173));
#15377=CARTESIAN_POINT('',(10.1999999975107,1.19856231453552,0.605472757505173));
#15378=CARTESIAN_POINT('Ctrl Pts',(10.1999999975107,1.19856231453552,0.605472757505173));
#15379=CARTESIAN_POINT('Ctrl Pts',(10.1999999975107,1.20410418062036,0.504502195294633));
#15380=CARTESIAN_POINT('Ctrl Pts',(10.2,1.20964514726505,0.403530798997214));
#15381=CARTESIAN_POINT('Ctrl Pts',(10.2,1.22071867750565,0.201707067365009));
#15382=CARTESIAN_POINT('Ctrl Pts',(10.2,1.22625132869937,0.100853170395858));
#15383=CARTESIAN_POINT('Ctrl Pts',(10.2,1.23178301601145,0.));
#15384=CARTESIAN_POINT('',(10.1999999980542,1.09857320530976,0.7));
#15385=CARTESIAN_POINT('Ctrl Pts',(10.1999999999973,1.09857320510493,0.7));
#15386=CARTESIAN_POINT('Ctrl Pts',(10.2000000008642,1.10649088744708,0.699999999248278));
#15387=CARTESIAN_POINT('Ctrl Pts',(10.1999989363772,1.11434529358656,0.699006164779054));
#15388=CARTESIAN_POINT('Ctrl Pts',(10.1999980093114,1.12199598895487,0.697118997523365));
#15389=CARTESIAN_POINT('Ctrl Pts',(10.1999974900707,1.12628106973794,0.696062013320951));
#15390=CARTESIAN_POINT('Ctrl Pts',(10.1999970168623,1.13050229860485,0.694723760583242));
#15391=CARTESIAN_POINT('Ctrl Pts',(10.199996713894,1.13463332887353,0.693115046692397));
#15392=CARTESIAN_POINT('Ctrl Pts',(10.1999961690675,1.14206214329588,0.690222103243312));
#15393=CARTESIAN_POINT('Ctrl Pts',(10.1999962772589,1.14911941279843,0.686488866209959));
#15394=CARTESIAN_POINT('Ctrl Pts',(10.1999969599022,1.15565885618684,0.681996408643444));
#15395=CARTESIAN_POINT('Ctrl Pts',(10.1999973343062,1.15924549304116,0.679532465931891));
#15396=CARTESIAN_POINT('Ctrl Pts',(10.1999978674396,1.16267609380848,0.676839263748528));
#15397=CARTESIAN_POINT('Ctrl Pts',(10.1999983417863,1.16592263776853,0.673924718551186));
#15398=CARTESIAN_POINT('Ctrl Pts',(10.199998806773,1.16910511991263,0.671067684066867));
#15399=CARTESIAN_POINT('Ctrl Pts',(10.1999992207276,1.17209141256199,0.668015240668471));
#15400=CARTESIAN_POINT('Ctrl Pts',(10.1999992206607,1.17485880184773,0.664778864469812));
#15401=CARTESIAN_POINT('Ctrl Pts',(10.1999992205369,1.17997899231675,0.658790960038769));
#15402=CARTESIAN_POINT('Ctrl Pts',(10.1999979581638,1.18435276586188,0.652174799271591));
#15403=CARTESIAN_POINT('Ctrl Pts',(10.1999975326045,1.18791964688485,0.645095405674036));
#15404=CARTESIAN_POINT('Ctrl Pts',(10.1999974898604,1.18827791229431,0.644384335742179));
#15405=CARTESIAN_POINT('Ctrl Pts',(10.1999974535047,1.18862799840101,0.643668573506599));
#15406=CARTESIAN_POINT('Ctrl Pts',(10.1999974242393,1.18896981696374,0.64294827577739));
#15407=CARTESIAN_POINT('Ctrl Pts',(10.1999971329942,1.1923715530028,0.635779961907205));
#15408=CARTESIAN_POINT('Ctrl Pts',(10.1999977790614,1.19491900203126,0.628247233077589));
#15409=CARTESIAN_POINT('Ctrl Pts',(10.1999987199397,1.19655829940385,0.620518158911201));
#15410=CARTESIAN_POINT('Ctrl Pts',(10.1999993222661,1.19760773597399,0.615570201805241));
#15411=CARTESIAN_POINT('Ctrl Pts',(10.2,1.19828413277105,0.610541112135461));
#15412=CARTESIAN_POINT('Ctrl Pts',(10.2,1.19856231427281,0.60547275750556));
#15413=CARTESIAN_POINT('',(10.2,-1.09857320510402,0.7));
#15414=CARTESIAN_POINT('',(10.2,-0.653773457742722,0.7));
#15415=CARTESIAN_POINT('Ctrl Pts',(10.2,-1.19856231427281,0.60547275750556));
#15416=CARTESIAN_POINT('Ctrl Pts',(10.2,-1.19812809376428,0.613384079828744));
#15417=CARTESIAN_POINT('Ctrl Pts',(10.1999984889428,-1.1967261327477,0.621202329970501));
#15418=CARTESIAN_POINT('Ctrl Pts',(10.1999978161146,-1.19444079525024,0.628767398200536));
#15419=CARTESIAN_POINT('Ctrl Pts',(10.1999974438306,-1.19317629038787,0.632953241898348));
#15420=CARTESIAN_POINT('Ctrl Pts',(10.1999972759003,-1.19164034846853,0.637061602680377));
#15421=CARTESIAN_POINT('Ctrl Pts',(10.1999973648938,-1.18984073583679,0.641063423920242));
#15422=CARTESIAN_POINT('Ctrl Pts',(10.1999975257516,-1.18658789218766,0.648296813248274));
#15423=CARTESIAN_POINT('Ctrl Pts',(10.1999986492083,-1.18251199594868,0.655103972585077));
#15424=CARTESIAN_POINT('Ctrl Pts',(10.1999990866637,-1.1776776067306,0.66132208754656));
#15425=CARTESIAN_POINT('Ctrl Pts',(10.1999991692372,-1.17676507450965,0.662495809810115));
#15426=CARTESIAN_POINT('Ctrl Pts',(10.1999992204458,-1.17582538639523,0.663648473741297));
#15427=CARTESIAN_POINT('Ctrl Pts',(10.1999992199672,-1.17485880188435,0.664778864469789));
#15428=CARTESIAN_POINT('Ctrl Pts',(10.1999992190419,-1.17299032792757,0.666963987046661));
#15429=CARTESIAN_POINT('Ctrl Pts',(10.1999990265713,-1.17102137903347,0.669065925022507));
#15430=CARTESIAN_POINT('Ctrl Pts',(10.1999987631451,-1.16895889720817,0.671081139337088));
#15431=CARTESIAN_POINT('Ctrl Pts',(10.1999980371048,-1.16327440276409,0.676635357771578));
#15432=CARTESIAN_POINT('Ctrl Pts',(10.1999968952367,-1.15694629605269,0.681471105251756));
#15433=CARTESIAN_POINT('Ctrl Pts',(10.1999965193249,-1.15013861030111,0.685534582868085));
#15434=CARTESIAN_POINT('Ctrl Pts',(10.1999962798276,-1.14580136285465,0.688123466749966));
#15435=CARTESIAN_POINT('Ctrl Pts',(10.1999963003895,-1.14126848503633,0.690398200126003));
#15436=CARTESIAN_POINT('Ctrl Pts',(10.1999965837416,-1.13657664085124,0.692335536714198));
#15437=CARTESIAN_POINT('Ctrl Pts',(10.199997026059,-1.12925259320479,0.695359751696499));
#15438=CARTESIAN_POINT('Ctrl Pts',(10.1999981114625,-1.12162598460505,0.697529439192009));
#15439=CARTESIAN_POINT('Ctrl Pts',(10.1999989867727,-1.11384404680861,0.698775198878229));
#15440=CARTESIAN_POINT('Ctrl Pts',(10.1999995533653,-1.10880676031141,0.699581585232154));
#15441=CARTESIAN_POINT('Ctrl Pts',(10.200000000559,-1.10370379302489,0.699999999512891));
#15442=CARTESIAN_POINT('Ctrl Pts',(10.1999999999973,-1.09857320510493,0.7));
#15443=CARTESIAN_POINT('Ctrl Pts',(10.0273290644374,-1.24073895154929,-0.000342977371441382));
#15444=CARTESIAN_POINT('Ctrl Pts',(10.0182194939277,-1.2301570933055,0.201590462913323));
#15445=CARTESIAN_POINT('Ctrl Pts',(10.0091098064739,-1.21957524432673,0.403523898419685));
#15446=CARTESIAN_POINT('Ctrl Pts',(10.,-1.20899340483173,0.605457329065658));
#15447=CARTESIAN_POINT('Ctrl Pts',(9.11786336174441,-1.287320026752,-0.000205293215301774));
#15448=CARTESIAN_POINT('Ctrl Pts',(9.11054075262461,-1.27673792859995,0.201728409731728));
#15449=CARTESIAN_POINT('Ctrl Pts',(9.10321803982027,-1.2661558351744,0.403662109352091));
#15450=CARTESIAN_POINT('Ctrl Pts',(9.09589522044064,-1.25557375159922,0.605595805683776));
#15451=CARTESIAN_POINT('Ctrl Pts',(8.20875307681921,-1.32613868191631,-8.19769783003664E-5));
#15452=CARTESIAN_POINT('Ctrl Pts',(8.20321812688803,-1.31555630757271,0.201851960079368));
#15453=CARTESIAN_POINT('Ctrl Pts',(8.19768309032111,-1.30497393555236,0.403785895133155));
#15454=CARTESIAN_POINT('Ctrl Pts',(8.19214796413157,-1.29439157095064,0.605719828258773));
#15455=CARTESIAN_POINT('Ctrl Pts',(7.29999999999999,-1.35236351479115,1.04083408558608E-17));
#15456=CARTESIAN_POINT('Ctrl Pts',(7.29625341766944,-1.34178092325774,0.201934092022114));
#15457=CARTESIAN_POINT('Ctrl Pts',(7.2925067690755,-1.33119833465137,0.403868182971915));
#15458=CARTESIAN_POINT('Ctrl Pts',(7.28876005303739,-1.32061574904145,0.605802272831199));
#15459=CARTESIAN_POINT('Ctrl Pts',(7.29999999953094,-1.32031613471704,0.605285370449856));
#15460=CARTESIAN_POINT('Ctrl Pts',(8.20058408060299,-1.29406305600824,0.605326635812744));
#15461=CARTESIAN_POINT('Ctrl Pts',(9.10058974048747,-1.25534320916473,0.605388449123016));
#15462=CARTESIAN_POINT('Ctrl Pts',(9.99999999968202,-1.20899340489109,0.605457329065633));
#15463=CARTESIAN_POINT('Ctrl Pts',(10.5052670937641,-1.21555282972197,-4.72190879230918E-5));
#15464=CARTESIAN_POINT('Ctrl Pts',(10.4952228315222,-1.20497561405085,0.201799837144789));
#15465=CARTESIAN_POINT('Ctrl Pts',(10.4851784461209,-1.19439840869387,0.403646887802288));
#15466=CARTESIAN_POINT('Ctrl Pts',(10.4751339353761,-1.18382121389426,0.605493932788863));
#15467=CARTESIAN_POINT('Ctrl Pts',(10.4035069533234,-1.22105168617584,-3.13467776074076E-5));
#15468=CARTESIAN_POINT('Ctrl Pts',(10.3936624949941,-1.21047444506522,0.201815739766394));
#15469=CARTESIAN_POINT('Ctrl Pts',(10.3838179147697,-1.19989721405033,0.403662820908308));
#15470=CARTESIAN_POINT('Ctrl Pts',(10.3739732104882,-1.18931999337004,0.605509896555428));
#15471=CARTESIAN_POINT('Ctrl Pts',(10.3017512542637,-1.22646400658821,-1.55943981238903E-5));
#15472=CARTESIAN_POINT('Ctrl Pts',(10.2921066085356,-1.21588673949083,0.201831522212972));
#15473=CARTESIAN_POINT('Ctrl Pts',(10.2824618422276,-1.20530948226626,0.403678633593635));
#15474=CARTESIAN_POINT('Ctrl Pts',(10.2728169532007,-1.19473223514815,0.605525739654126));
#15475=CARTESIAN_POINT('Ctrl Pts',(10.2,-1.23178301601145,-4.5102810375397E-17));
#15476=CARTESIAN_POINT('Ctrl Pts',(10.1905551755811,-1.22120572247414,0.20184714636246));
#15477=CARTESIAN_POINT('Ctrl Pts',(10.1811102319487,-1.21062843858304,0.403694287664275));
#15478=CARTESIAN_POINT('Ctrl Pts',(10.1716651669877,-1.20005116456574,0.605541423818621));
#15479=CARTESIAN_POINT('',(10.4735630903435,-1.18390659316268,0.605494180667944));
#15480=CARTESIAN_POINT('Ctrl Pts',(10.1999999975038,-1.19856231440453,0.605472757505366));
#15481=CARTESIAN_POINT('Ctrl Pts',(10.2911933328565,-1.19375025772558,0.605479840815741));
#15482=CARTESIAN_POINT('Ctrl Pts',(10.3823809652617,-1.18886335120032,0.605486986548286));
#15483=CARTESIAN_POINT('Ctrl Pts',(10.4735630903435,-1.18390659316268,0.605494180667944));
#15484=CARTESIAN_POINT('Ctrl Pts',(10.4735630903435,-1.18390659316268,0.605494180667945));
#15485=CARTESIAN_POINT('Ctrl Pts',(10.4841302498201,-1.19445434834508,0.403662775875149));
#15486=CARTESIAN_POINT('Ctrl Pts',(10.4946974680575,-1.20500226999407,0.201831382381129));
#15487=CARTESIAN_POINT('Ctrl Pts',(10.5052647440597,-1.21555035534119,-6.86299975183324E-17));
#15488=CARTESIAN_POINT('Ctrl Pts',(10.,-1.10900986674273,0.7));
#15489=CARTESIAN_POINT('Ctrl Pts',(9.09944331332257,-1.15544418981837,0.7));
#15490=CARTESIAN_POINT('Ctrl Pts',(8.1984670949788,-1.19422430779862,0.7));
#15491=CARTESIAN_POINT('Ctrl Pts',(7.29709043526679,-1.22049830417059,0.7));
#15492=CARTESIAN_POINT('Ctrl Pts',(10.0014871213396,-1.13785139984992,0.7));
#15493=CARTESIAN_POINT('Ctrl Pts',(9.10076698492608,-1.18430758604571,0.700000491839571));
#15494=CARTESIAN_POINT('Ctrl Pts',(8.19957769811723,-1.22310890030201,0.699999704549177));
#15495=CARTESIAN_POINT('Ctrl Pts',(7.29793284700475,-1.24939875264889,0.7));
#15496=CARTESIAN_POINT('Ctrl Pts',(10.0040646682326,-1.18784086746588,0.676686753673613));
#15497=CARTESIAN_POINT('Ctrl Pts',(9.10306300621911,-1.23433322993607,0.676664155483858));
#15498=CARTESIAN_POINT('Ctrl Pts',(8.20149954052229,-1.27317186922949,0.676644146017133));
#15499=CARTESIAN_POINT('Ctrl Pts',(7.29939288958795,-1.29948813715084,0.676630595533454));
#15500=CARTESIAN_POINT('Ctrl Pts',(10.0050807923581,-1.20754778500352,0.627085325222079));
#15501=CARTESIAN_POINT('Ctrl Pts',(9.10396596140607,-1.25402923300358,0.627026849623412));
#15502=CARTESIAN_POINT('Ctrl Pts',(8.20225661204673,-1.29285896783792,0.626974637782525));
#15503=CARTESIAN_POINT('Ctrl Pts',(7.29996660609514,-1.31917051289423,0.626939603849942));
#15504=CARTESIAN_POINT('Ctrl Pts',(10.0051416645797,-1.20872835322339,0.605457722909465));
#15505=CARTESIAN_POINT('Ctrl Pts',(9.1040197884667,-1.25519559703033,0.605388684776982));
#15506=CARTESIAN_POINT('Ctrl Pts',(8.20230020786566,-1.29401302889245,0.605326714446839));
#15507=CARTESIAN_POINT('Ctrl Pts',(7.29999999953094,-1.32031613471704,0.605285370449856));
#15508=CARTESIAN_POINT('Ctrl Pts',(10.4681436286308,-1.08420482079362,0.7));
#15509=CARTESIAN_POINT('Ctrl Pts',(10.3770124662346,-1.0891584122264,0.7));
#15510=CARTESIAN_POINT('Ctrl Pts',(10.285877616441,-1.09404209584202,0.7));
#15511=CARTESIAN_POINT('Ctrl Pts',(10.1947388861048,-1.09885088260188,0.7));
#15512=CARTESIAN_POINT('Ctrl Pts',(10.4697107510168,-1.11303515260326,0.7));
#15513=CARTESIAN_POINT('Ctrl Pts',(10.3785648662465,-1.11799094453753,0.700000051218742));
#15514=CARTESIAN_POINT('Ctrl Pts',(10.2874149314686,-1.12287675076168,0.699999949550842));
#15515=CARTESIAN_POINT('Ctrl Pts',(10.196260416419,-1.12768774893097,0.7));
#15516=CARTESIAN_POINT('Ctrl Pts',(10.4724269697127,-1.16300539549315,0.676698381019543));
#15517=CARTESIAN_POINT('Ctrl Pts',(10.3812557252598,-1.16796482352885,0.676696026813929));
#15518=CARTESIAN_POINT('Ctrl Pts',(10.2900793016129,-1.17285439035486,0.676693724638983));
#15519=CARTESIAN_POINT('Ctrl Pts',(10.1988975981852,-1.17766904563614,0.67669140632491));
#15520=CARTESIAN_POINT('Ctrl Pts',(10.4734985149421,-1.18271860027509,0.627116141711795));
#15521=CARTESIAN_POINT('Ctrl Pts',(10.382317043787,-1.18767684023183,0.627110048826767));
#15522=CARTESIAN_POINT('Ctrl Pts',(10.2911301919381,-1.19256517083271,0.627104033151799));
#15523=CARTESIAN_POINT('Ctrl Pts',(10.1999375452555,-1.19737868557977,0.627098033786781));
#15524=CARTESIAN_POINT('Ctrl Pts',(10.4735630903435,-1.18390659316268,0.605494180667944));
#15525=CARTESIAN_POINT('Ctrl Pts',(10.3823809652617,-1.18886335120032,0.605486986548286));
#15526=CARTESIAN_POINT('Ctrl Pts',(10.2911933328565,-1.19375025772558,0.605479840815741));
#15527=CARTESIAN_POINT('Ctrl Pts',(10.1999999975038,-1.19856231440453,0.605472757505366));
#15528=CARTESIAN_POINT('',(10.4681436258201,-1.08420482094639,0.7));
#15529=CARTESIAN_POINT('Ctrl Pts',(10.4681436258201,-1.0842048209464,0.7));
#15530=CARTESIAN_POINT('Ctrl Pts',(10.3787660248044,-1.08906309452597,0.7));
#15531=CARTESIAN_POINT('Ctrl Pts',(10.289384876933,-1.09385412476048,0.7));
#15532=CARTESIAN_POINT('Ctrl Pts',(10.1999999999973,-1.09857320510493,0.7));
#15533=CARTESIAN_POINT('Origin',(10.4681436286308,-1.08420482099672,0.6));
#15534=CARTESIAN_POINT('Origin',(5.4,-8.11656130105013E-18,0.7));
#15535=CARTESIAN_POINT('',(10.4681436286308,1.08420482109828,0.7));
#15536=CARTESIAN_POINT('Ctrl Pts',(10.1999999980461,1.09857320520795,0.7));
#15537=CARTESIAN_POINT('Ctrl Pts',(10.2893848765692,1.09385412478074,0.7));
#15538=CARTESIAN_POINT('Ctrl Pts',(10.3787660260279,1.08906309446088,0.7));
#15539=CARTESIAN_POINT('Ctrl Pts',(10.4681436286308,1.08420482079361,0.7));
#15540=CARTESIAN_POINT('',(10.4681436286308,0.7,0.7));
#15541=CARTESIAN_POINT('Ctrl Pts',(7.3,1.35236351479305,-3.57463069561303E-11));
#15542=CARTESIAN_POINT('Ctrl Pts',(7.29625341766908,1.34178092325856,0.20193409200674));
#15543=CARTESIAN_POINT('Ctrl Pts',(7.29250676907475,1.33119833465113,0.403868182976914));
#15544=CARTESIAN_POINT('Ctrl Pts',(7.28876005303626,1.32061574904014,0.60580227285657));
#15545=CARTESIAN_POINT('Ctrl Pts',(8.20875307682014,1.32613868191819,-8.19770140467192E-5));
#15546=CARTESIAN_POINT('Ctrl Pts',(8.20321812688841,1.31555630757352,0.201851960063995));
#15547=CARTESIAN_POINT('Ctrl Pts',(8.19768309032092,1.3049739355521,0.403785895138154));
#15548=CARTESIAN_POINT('Ctrl Pts',(8.19214796413082,1.29439157094932,0.605719828284144));
#15549=CARTESIAN_POINT('Ctrl Pts',(9.11786336174626,1.28732002675385,-0.000205293251048056));
#15550=CARTESIAN_POINT('Ctrl Pts',(9.11054075262572,1.27673792860073,0.201728409716354));
#15551=CARTESIAN_POINT('Ctrl Pts',(9.10321803982063,1.26615583517412,0.403662109357089));
#15552=CARTESIAN_POINT('Ctrl Pts',(9.09589522044026,1.25557375159787,0.605595805709147));
#15553=CARTESIAN_POINT('Ctrl Pts',(10.0273290644402,1.2407389515511,-0.000342977407187712));
#15554=CARTESIAN_POINT('Ctrl Pts',(10.0182194939295,1.23015709330624,0.201590462897949));
#15555=CARTESIAN_POINT('Ctrl Pts',(10.0091098064748,1.21957524432641,0.403523898424684));
#15556=CARTESIAN_POINT('Ctrl Pts',(10.,1.20899340483035,0.605457329091028));
#15557=CARTESIAN_POINT('Ctrl Pts',(10.2,1.23178301601276,-2.39624899783797E-11));
#15558=CARTESIAN_POINT('Ctrl Pts',(10.1905551755807,1.22120572247504,0.201847146346486));
#15559=CARTESIAN_POINT('Ctrl Pts',(10.1811102319479,1.21062843858352,0.403694287656288));
#15560=CARTESIAN_POINT('Ctrl Pts',(10.1716651669865,1.2000511645658,0.605541423818621));
#15561=CARTESIAN_POINT('Ctrl Pts',(10.3017512542641,1.22646400658951,-1.55944220863836E-5));
#15562=CARTESIAN_POINT('Ctrl Pts',(10.2921066085356,1.2158867394917,0.201831522196997));
#15563=CARTESIAN_POINT('Ctrl Pts',(10.2824618422272,1.20530948226672,0.403678633585648));
#15564=CARTESIAN_POINT('Ctrl Pts',(10.2728169531999,1.19473223514819,0.605525739654127));
#15565=CARTESIAN_POINT('Ctrl Pts',(10.4035069533242,1.22105168617711,-3.13468015701665E-5));
#15566=CARTESIAN_POINT('Ctrl Pts',(10.3936624949945,1.21047444506608,0.201815739750419));
#15567=CARTESIAN_POINT('Ctrl Pts',(10.3838179147698,1.19989721405077,0.40366282090032));
#15568=CARTESIAN_POINT('Ctrl Pts',(10.3739732104878,1.18931999337006,0.605509896555428));
#15569=CARTESIAN_POINT('Ctrl Pts',(10.5052670937653,1.21555282972323,-4.72191118859062E-5));
#15570=CARTESIAN_POINT('Ctrl Pts',(10.495222831523,1.20497561405169,0.201799837128814));
#15571=CARTESIAN_POINT('Ctrl Pts',(10.4851784461213,1.19439840869429,0.403646887794301));
#15572=CARTESIAN_POINT('Ctrl Pts',(10.4751339353761,1.18382121389426,0.605493932788864));
#15573=CARTESIAN_POINT('',(10.4735630903435,1.18390659316268,0.605494180667944));
#15574=CARTESIAN_POINT('Ctrl Pts',(10.5052647440597,1.21555035534119,-4.0462425077159E-16));
#15575=CARTESIAN_POINT('Ctrl Pts',(10.4946974680575,1.20500226999407,0.201831382381129));
#15576=CARTESIAN_POINT('Ctrl Pts',(10.4841302498201,1.19445434834508,0.40366277587515));
#15577=CARTESIAN_POINT('Ctrl Pts',(10.4735630903435,1.18390659316268,0.605494180667945));
#15578=CARTESIAN_POINT('Ctrl Pts',(10.4735630903435,1.18390659316268,0.605494180667944));
#15579=CARTESIAN_POINT('Ctrl Pts',(10.3823809652617,1.18886335120032,0.605486986548286));
#15580=CARTESIAN_POINT('Ctrl Pts',(10.2911933328565,1.19375025772558,0.605479840815741));
#15581=CARTESIAN_POINT('Ctrl Pts',(10.1999999975038,1.19856231440453,0.605472757505366));
#15582=CARTESIAN_POINT('Origin',(7.1,1.42555555555556,0.));
#15583=CARTESIAN_POINT('',(7.0999999994629,-1.32593912634735,0.605276549957215));
#15584=CARTESIAN_POINT('Ctrl Pts',(7.0999999994629,-1.32593912634735,0.605276549957215));
#15585=CARTESIAN_POINT('Ctrl Pts',(7.0999999994629,-1.33126650931098,0.504490734647167));
#15586=CARTESIAN_POINT('Ctrl Pts',(7.1,-1.33659376385849,0.403703958452373));
#15587=CARTESIAN_POINT('Ctrl Pts',(7.1,-1.3472576786761,0.201945747207886));
#15588=CARTESIAN_POINT('Ctrl Pts',(7.1,-1.35259443928223,0.100972400854069));
#15589=CARTESIAN_POINT('Ctrl Pts',(7.1,-1.35793097395724,0.));
#15590=CARTESIAN_POINT('',(7.1,-1.22604182196417,0.7));
#15591=CARTESIAN_POINT('Ctrl Pts',(7.1,-1.22604182196307,0.7));
#15592=CARTESIAN_POINT('Ctrl Pts',(7.1,-1.23395163718705,0.7));
#15593=CARTESIAN_POINT('Ctrl Pts',(7.09999945440688,-1.24179783218049,0.699006056038995));
#15594=CARTESIAN_POINT('Ctrl Pts',(7.09999897931553,-1.2494401870438,0.697119011207626));
#15595=CARTESIAN_POINT('Ctrl Pts',(7.09999871186578,-1.25374240366384,0.696056710937424));
#15596=CARTESIAN_POINT('Ctrl Pts',(7.09999846845149,-1.25798007942473,0.69471034534287));
#15597=CARTESIAN_POINT('Ctrl Pts',(7.09999831430822,-1.26212651101681,0.6930909329195));
#15598=CARTESIAN_POINT('Ctrl Pts',(7.09999803835695,-1.26954956016987,0.690191818885951));
#15599=CARTESIAN_POINT('Ctrl Pts',(7.09999810102228,-1.27659977900265,0.686452252582521));
#15600=CARTESIAN_POINT('Ctrl Pts',(7.09999845706054,-1.28313109767173,0.681953977461377));
#15601=CARTESIAN_POINT('Ctrl Pts',(7.09999865314126,-1.2867280867584,0.679476645189077));
#15602=CARTESIAN_POINT('Ctrl Pts',(7.09999893113315,-1.29016742765117,0.67676830886676));
#15603=CARTESIAN_POINT('Ctrl Pts',(7.09999917787259,-1.2934208019838,0.673837071833988));
#15604=CARTESIAN_POINT('Ctrl Pts',(7.09999941835505,-1.29659167515528,0.670980166997299));
#15605=CARTESIAN_POINT('Ctrl Pts',(7.09999963169439,-1.29956664557352,0.667928795646746));
#15606=CARTESIAN_POINT('Ctrl Pts',(7.09999963110542,-1.30232317314677,0.664694459428825));
#15607=CARTESIAN_POINT('Ctrl Pts',(7.09999963001387,-1.30743194453681,0.658700148145236));
#15608=CARTESIAN_POINT('Ctrl Pts',(7.09999897381858,-1.31179333085743,0.652078782729069));
#15609=CARTESIAN_POINT('Ctrl Pts',(7.09999874753952,-1.31534789998199,0.64499600756552));
#15610=CARTESIAN_POINT('Ctrl Pts',(7.09999872438549,-1.31571162172319,0.644271261689237));
#15611=CARTESIAN_POINT('Ctrl Pts',(7.0999987046402,-1.31606685549941,0.643541664816448));
#15612=CARTESIAN_POINT('Ctrl Pts',(7.09999868869212,-1.31641350913238,0.642807383257706));
#15613=CARTESIAN_POINT('Ctrl Pts',(7.09999853283271,-1.31980133087414,0.635631300872562));
#15614=CARTESIAN_POINT('Ctrl Pts',(7.09999885939544,-1.32233451509485,0.628092322434426));
#15615=CARTESIAN_POINT('Ctrl Pts',(7.09999934101855,-1.32395982399511,0.620358959365968));
#15616=CARTESIAN_POINT('Ctrl Pts',(7.09999964997549,-1.32500244522074,0.615398075635307));
#15617=CARTESIAN_POINT('Ctrl Pts',(7.09999999934316,-1.32567060646853,0.610356529630438));
#15618=CARTESIAN_POINT('Ctrl Pts',(7.09999999981141,-1.32593912630714,0.60527654995744));
#15619=CARTESIAN_POINT('',(7.09999999995537,1.22604182196549,0.7));
#15620=CARTESIAN_POINT('',(7.1,0.712777777777778,0.7));
#15621=CARTESIAN_POINT('',(7.0999999994629,1.32593912634735,0.605276549957215));
#15622=CARTESIAN_POINT('Ctrl Pts',(7.09999999981142,1.32593912630714,0.60527654995744));
#15623=CARTESIAN_POINT('Ctrl Pts',(7.09999999908198,1.32552083177145,0.613190035045322));
#15624=CARTESIAN_POINT('Ctrl Pts',(7.09999922367565,1.32413525001942,0.621012727860624));
#15625=CARTESIAN_POINT('Ctrl Pts',(7.09999888117586,1.32186630199077,0.628584136488803));
#15626=CARTESIAN_POINT('Ctrl Pts',(7.09999868987568,1.32059900146923,0.632813078704371));
#15627=CARTESIAN_POINT('Ctrl Pts',(7.09999860640034,1.3190551184949,0.636963663611311));
#15628=CARTESIAN_POINT('Ctrl Pts',(7.09999865766138,1.31724253497577,0.641005923298765));
#15629=CARTESIAN_POINT('Ctrl Pts',(7.0999987494091,1.31399834762864,0.648240816253195));
#15630=CARTESIAN_POINT('Ctrl Pts',(7.09999933613984,1.30993159792479,0.655050690394837));
#15631=CARTESIAN_POINT('Ctrl Pts',(7.09999956222935,1.30510592187917,0.661272231165006));
#15632=CARTESIAN_POINT('Ctrl Pts',(7.09999960444598,1.30420484616769,0.662433950108221));
#15633=CARTESIAN_POINT('Ctrl Pts',(7.09999963060969,1.30327718139331,0.663575086117144));
#15634=CARTESIAN_POINT('Ctrl Pts',(7.09999963056866,1.30232317316131,0.664694459428815));
#15635=CARTESIAN_POINT('Ctrl Pts',(7.09999963048683,1.30042028596585,0.666927187690779));
#15636=CARTESIAN_POINT('Ctrl Pts',(7.09999952705857,1.29841262431024,0.669073382394206));
#15637=CARTESIAN_POINT('Ctrl Pts',(7.09999938633452,1.29630755303174,0.671129253595323));
#15638=CARTESIAN_POINT('Ctrl Pts',(7.09999900634735,1.29062337821964,0.676680576924663));
#15639=CARTESIAN_POINT('Ctrl Pts',(7.09999841760642,1.2842958957007,0.681513596217188));
#15640=CARTESIAN_POINT('Ctrl Pts',(7.0999982224057,1.2774887935492,0.68557385059291));
#15641=CARTESIAN_POINT('Ctrl Pts',(7.09999809840912,1.27316474526651,0.688153029745784));
#15642=CARTESIAN_POINT('Ctrl Pts',(7.09999810738417,1.26864620899217,0.690419707112974));
#15643=CARTESIAN_POINT('Ctrl Pts',(7.09999825155258,1.26396949224645,0.69235064530212));
#15644=CARTESIAN_POINT('Ctrl Pts',(7.09999847710269,1.25665281355793,0.695371579659609));
#15645=CARTESIAN_POINT('Ctrl Pts',(7.09999903441007,1.2490339950321,0.697538299034574));
#15646=CARTESIAN_POINT('Ctrl Pts',(7.09999948258254,1.24125996729125,0.698781081437474));
#15647=CARTESIAN_POINT('Ctrl Pts',(7.09999977198436,1.23623998534067,0.699583592753232));
#15648=CARTESIAN_POINT('Ctrl Pts',(7.1,1.23115469319345,0.7));
#15649=CARTESIAN_POINT('Ctrl Pts',(7.1,1.22604182196307,0.7));
#15650=CARTESIAN_POINT('Ctrl Pts',(7.1,1.35793097395724,0.));
#15651=CARTESIAN_POINT('Ctrl Pts',(7.1,1.35259441576718,0.100972845781549));
#15652=CARTESIAN_POINT('Ctrl Pts',(7.1,1.34725763161617,0.201946637598055));
#15653=CARTESIAN_POINT('Ctrl Pts',(7.1,1.33659371676552,0.403704849408333));
#15654=CARTESIAN_POINT('Ctrl Pts',(7.0999999994629,1.33126648576411,0.504491180117376));
#15655=CARTESIAN_POINT('Ctrl Pts',(7.0999999994629,1.32593912634735,0.605276549957215));
#15656=CARTESIAN_POINT('Ctrl Pts',(7.11011156210589,-1.35766432821499,-9.27062925672982E-5));
#15657=CARTESIAN_POINT('Ctrl Pts',(7.10674110347764,-1.34708925835705,0.201697046690488));
#15658=CARTESIAN_POINT('Ctrl Pts',(7.10337058314201,-1.33651419103807,0.403486798779133));
#15659=CARTESIAN_POINT('Ctrl Pts',(7.09999999999996,-1.32593912631822,0.605276549958221));
#15660=CARTESIAN_POINT('Ctrl Pts',(5.9694837631095,-1.38835096090528,2.80675674898241E-6));
#15661=CARTESIAN_POINT('Ctrl Pts',(5.96835662351021,-1.37777563343505,0.201792740207853));
#15662=CARTESIAN_POINT('Ctrl Pts',(5.96722945517891,-1.3672003004237,0.40358267322573));
#15663=CARTESIAN_POINT('Ctrl Pts',(5.96610224583462,-1.35662497356325,0.605372606931572));
#15664=CARTESIAN_POINT('Ctrl Pts',(4.8294200007394,-1.39866452387306,3.01102374082134E-5));
#15665=CARTESIAN_POINT('Ctrl Pts',(4.83053730380309,-1.38808904115766,0.201820093264151));
#15666=CARTESIAN_POINT('Ctrl Pts',(4.83165461298617,-1.3775135517806,0.403610075973038));
#15667=CARTESIAN_POINT('Ctrl Pts',(4.83277191472125,-1.36693806692183,0.605400059795761));
#15668=CARTESIAN_POINT('Ctrl Pts',(3.68991216363982,-1.37907703205181,-6.2684699445455E-5));
#15669=CARTESIAN_POINT('Ctrl Pts',(3.69327498756969,-1.36850179198701,0.201727122618256));
#15670=CARTESIAN_POINT('Ctrl Pts',(3.69663785098144,-1.3579265529724,0.403516929334346));
#15671=CARTESIAN_POINT('Ctrl Pts',(3.70000075457889,-1.34735131503281,0.605306735438421));
#15672=CARTESIAN_POINT('Ctrl Pts',(3.69999999992215,-1.34735368792773,0.6052614572053));
#15673=CARTESIAN_POINT('Ctrl Pts',(4.83355316856959,-1.366961322855,0.605214762857233));
#15674=CARTESIAN_POINT('Ctrl Pts',(5.96724522208681,-1.35660163688233,0.605228569880684));
#15675=CARTESIAN_POINT('Ctrl Pts',(7.09999999927392,-1.32593912632169,0.605276549957417));
#15676=CARTESIAN_POINT('Ctrl Pts',(7.1,-1.22604182196307,0.7));
#15677=CARTESIAN_POINT('Ctrl Pts',(5.96696284938742,-1.25674179781664,0.7));
#15678=CARTESIAN_POINT('Ctrl Pts',(4.83327074934872,-1.26710800714677,0.7));
#15679=CARTESIAN_POINT('Ctrl Pts',(3.7,-1.24747724070879,0.7));
#15680=CARTESIAN_POINT('Ctrl Pts',(7.10078315634008,-1.25494559805327,0.7));
#15681=CARTESIAN_POINT('Ctrl Pts',(5.96739926106349,-1.28566432005869,0.700000343763215));
#15682=CARTESIAN_POINT('Ctrl Pts',(4.83328164159484,-1.29603890521481,0.700000334703603));
#15683=CARTESIAN_POINT('Ctrl Pts',(3.69949916377151,-1.27639017438114,0.7));
#15684=CARTESIAN_POINT('Ctrl Pts',(7.10214055788579,-1.30504291366416,0.676629771601708));
#15685=CARTESIAN_POINT('Ctrl Pts',(5.96815960929481,-1.33579288254824,0.676614006760374));
#15686=CARTESIAN_POINT('Ctrl Pts',(4.83329467960724,-1.3461818279488,0.676609489640654));
#15687=CARTESIAN_POINT('Ctrl Pts',(3.69863109538965,-1.3265031696486,0.676624836591801));
#15688=CARTESIAN_POINT('Ctrl Pts',(7.10267376869946,-1.32472200604796,0.626932241521275));
#15689=CARTESIAN_POINT('Ctrl Pts',(5.9684558952243,-1.35546668061705,0.626891484245174));
#15690=CARTESIAN_POINT('Ctrl Pts',(4.83330292199863,-1.36585610284781,0.626879766983475));
#15691=CARTESIAN_POINT('Ctrl Pts',(3.69829020046733,-1.34618280086838,0.626919440930842));
#15692=CARTESIAN_POINT('Ctrl Pts',(7.10270476209941,-1.32586587253612,0.605276664588022));
#15693=CARTESIAN_POINT('Ctrl Pts',(5.96847377630401,-1.35660073810322,0.605228567467576));
#15694=CARTESIAN_POINT('Ctrl Pts',(4.8333022084086,-1.36698748587873,0.605214711607465));
#15695=CARTESIAN_POINT('Ctrl Pts',(3.69827043673666,-1.34732374755196,0.60526152849799));
#15696=CARTESIAN_POINT('Ctrl Pts',(7.1,-1.22604182196307,0.7));
#15697=CARTESIAN_POINT('Ctrl Pts',(5.96696284938742,-1.25674179781664,0.7));
#15698=CARTESIAN_POINT('Ctrl Pts',(4.83327074934872,-1.26710800714677,0.7));
#15699=CARTESIAN_POINT('Ctrl Pts',(3.7,-1.24747724070879,0.7));
#15700=CARTESIAN_POINT('Origin',(5.4,-8.11656130105013E-18,0.7));
#15701=CARTESIAN_POINT('Ctrl Pts',(3.7,1.24747724070879,0.7));
#15702=CARTESIAN_POINT('Ctrl Pts',(4.83327074934871,1.26710800714677,0.7));
#15703=CARTESIAN_POINT('Ctrl Pts',(5.96696284938742,1.25674179781664,0.7));
#15704=CARTESIAN_POINT('Ctrl Pts',(7.1,1.22604182196307,0.7));
#15705=CARTESIAN_POINT('Ctrl Pts',(3.7,1.24747724070879,0.7));
#15706=CARTESIAN_POINT('Ctrl Pts',(4.83327074934871,1.26710800714677,0.7));
#15707=CARTESIAN_POINT('Ctrl Pts',(5.96696284938742,1.25674179781664,0.7));
#15708=CARTESIAN_POINT('Ctrl Pts',(7.1,1.22604182196307,0.7));
#15709=CARTESIAN_POINT('Ctrl Pts',(3.69949916377151,1.27639017438114,0.7));
#15710=CARTESIAN_POINT('Ctrl Pts',(4.83328164159484,1.29603890521481,0.700000334703603));
#15711=CARTESIAN_POINT('Ctrl Pts',(5.96739926106349,1.28566432005869,0.700000343763215));
#15712=CARTESIAN_POINT('Ctrl Pts',(7.10078315634008,1.25494559805327,0.7));
#15713=CARTESIAN_POINT('Ctrl Pts',(3.69863109538965,1.3265031696486,0.676624836591801));
#15714=CARTESIAN_POINT('Ctrl Pts',(4.83329467960724,1.3461818279488,0.676609489640654));
#15715=CARTESIAN_POINT('Ctrl Pts',(5.9681596092948,1.33579288254824,0.676614006760374));
#15716=CARTESIAN_POINT('Ctrl Pts',(7.10214055788579,1.30504291366416,0.676629771601707));
#15717=CARTESIAN_POINT('Ctrl Pts',(3.69829020046733,1.34618280086838,0.626919440930842));
#15718=CARTESIAN_POINT('Ctrl Pts',(4.83330292199863,1.36585610284781,0.626879766983475));
#15719=CARTESIAN_POINT('Ctrl Pts',(5.9684558952243,1.35546668061705,0.626891484245174));
#15720=CARTESIAN_POINT('Ctrl Pts',(7.10267376869946,1.32472200604796,0.626932241521275));
#15721=CARTESIAN_POINT('Ctrl Pts',(3.69827043673666,1.34732374755196,0.60526152849799));
#15722=CARTESIAN_POINT('Ctrl Pts',(4.83330220840859,1.36698748587873,0.605214711607465));
#15723=CARTESIAN_POINT('Ctrl Pts',(5.96847377630401,1.35660073810322,0.605228567467576));
#15724=CARTESIAN_POINT('Ctrl Pts',(7.10270476209941,1.32586587253612,0.605276664588022));
#15725=CARTESIAN_POINT('Ctrl Pts',(7.09999999927392,1.32593912632169,0.605276549957417));
#15726=CARTESIAN_POINT('Ctrl Pts',(5.96724522208681,1.35660163688233,0.605228569880684));
#15727=CARTESIAN_POINT('Ctrl Pts',(4.83355316856959,1.366961322855,0.605214762857233));
#15728=CARTESIAN_POINT('Ctrl Pts',(3.69999999992215,1.34735368792773,0.6052614572053));
#15729=CARTESIAN_POINT('Ctrl Pts',(3.68991216360307,1.37907703216746,-6.26869063400631E-5));
#15730=CARTESIAN_POINT('Ctrl Pts',(3.6932749875452,1.36850179206412,0.201727121146993));
#15731=CARTESIAN_POINT('Ctrl Pts',(3.69663785096921,1.35792655301095,0.403516928598715));
#15732=CARTESIAN_POINT('Ctrl Pts',(3.70000075457892,1.34735131503281,0.605306735438421));
#15733=CARTESIAN_POINT('Ctrl Pts',(4.8294200007272,1.39866452398872,3.01080305115927E-5));
#15734=CARTESIAN_POINT('Ctrl Pts',(4.83053730379496,1.38808904123477,0.201820091792887));
#15735=CARTESIAN_POINT('Ctrl Pts',(4.83165461298211,1.37751355181915,0.403610075237406));
#15736=CARTESIAN_POINT('Ctrl Pts',(4.83277191472127,1.36693806692183,0.605400059795761));
#15737=CARTESIAN_POINT('Ctrl Pts',(5.96948376312183,1.38835096102094,2.80454985295556E-6));
#15738=CARTESIAN_POINT('Ctrl Pts',(5.96835662351844,1.37777563351215,0.201792738736588));
#15739=CARTESIAN_POINT('Ctrl Pts',(5.96722945518303,1.36720030046225,0.403582672490098));
#15740=CARTESIAN_POINT('Ctrl Pts',(5.96610224583462,1.35662497356325,0.605372606931572));
#15741=CARTESIAN_POINT('Ctrl Pts',(7.11011156214274,1.35766432833065,-9.27084994613511E-5));
#15742=CARTESIAN_POINT('Ctrl Pts',(7.10674110350221,1.34708925843416,0.201697045219225));
#15743=CARTESIAN_POINT('Ctrl Pts',(7.10337058315429,1.33651419107662,0.403486798043502));
#15744=CARTESIAN_POINT('Ctrl Pts',(7.09999999999996,1.32593912631822,0.605276549958221));
#15745=CARTESIAN_POINT('Origin',(3.5,1.44777777777778,0.));
#15746=CARTESIAN_POINT('',(3.5,-1.34358136363184,0.605270327458634));
#15747=CARTESIAN_POINT('Ctrl Pts',(3.5,-1.34358136363184,0.605270327458634));
#15748=CARTESIAN_POINT('Ctrl Pts',(3.5,-1.34890136370362,0.504489156176152));
#15749=CARTESIAN_POINT('Ctrl Pts',(3.5,-1.35422123464986,0.403706701640381));
#15750=CARTESIAN_POINT('Ctrl Pts',(3.5,-1.3648706701715,0.201950780690867));
#15751=CARTESIAN_POINT('Ctrl Pts',(3.5,-1.3702003690246,0.100974756199658));
#15752=CARTESIAN_POINT('Ctrl Pts',(3.5,-1.37552980833516,0.));
#15753=CARTESIAN_POINT('',(3.5,-1.24369946473884,0.7));
#15754=CARTESIAN_POINT('Ctrl Pts',(3.49999999991873,-1.24369946470729,0.7));
#15755=CARTESIAN_POINT('Ctrl Pts',(3.49999999896975,-1.25160831520001,0.699999999810925));
#15756=CARTESIAN_POINT('Ctrl Pts',(3.50000040534574,-1.25945374057332,0.69900619751828));
#15757=CARTESIAN_POINT('Ctrl Pts',(3.50000075715473,-1.26709539726361,0.697119355224275));
#15758=CARTESIAN_POINT('Ctrl Pts',(3.5000009551612,-1.27139630362835,0.696057395447694));
#15759=CARTESIAN_POINT('Ctrl Pts',(3.50000113454144,-1.27563271975905,0.694711510656402));
#15760=CARTESIAN_POINT('Ctrl Pts',(3.50000124621709,-1.27977793997275,0.693092697679401));
#15761=CARTESIAN_POINT('Ctrl Pts',(3.50000144618968,-1.28720060051191,0.690193961644836));
#15762=CARTESIAN_POINT('Ctrl Pts',(3.50000138985083,-1.29425038514255,0.686454755369034));
#15763=CARTESIAN_POINT('Ctrl Pts',(3.5000011147959,-1.30078112659466,0.681956784255818));
#15764=CARTESIAN_POINT('Ctrl Pts',(3.50000096334461,-1.30437709646577,0.679480102439082));
#15765=CARTESIAN_POINT('Ctrl Pts',(3.50000075087427,-1.30781543681835,0.676772489296601));
#15766=CARTESIAN_POINT('Ctrl Pts',(3.50000056308077,-1.31106783354026,0.67384203444854));
#15767=CARTESIAN_POINT('Ctrl Pts',(3.50000037990614,-1.31424023611357,0.670983655445047));
#15768=CARTESIAN_POINT('Ctrl Pts',(3.50000021841608,-1.31721646102264,0.667930553458483));
#15769=CARTESIAN_POINT('Ctrl Pts',(3.50000022028926,-1.3199739184757,0.664694242102541));
#15770=CARTESIAN_POINT('Ctrl Pts',(3.50000022375892,-1.32508151834405,0.658699667848218));
#15771=CARTESIAN_POINT('Ctrl Pts',(3.50000072745304,-1.32944146850927,0.652077914129702));
#15772=CARTESIAN_POINT('Ctrl Pts',(3.50000090782832,-1.33299465793893,0.64499486611401));
#15773=CARTESIAN_POINT('Ctrl Pts',(3.50000092626355,-1.33335781125732,0.644270944003422));
#15774=CARTESIAN_POINT('Ctrl Pts',(3.50000094214549,-1.33371249714824,0.643542183465449));
#15775=CARTESIAN_POINT('Ctrl Pts',(3.5000009551778,-1.33405862411533,0.642808750463418));
#15776=CARTESIAN_POINT('Ctrl Pts',(3.50000108270827,-1.3374457225345,0.635631587173848));
#15777=CARTESIAN_POINT('Ctrl Pts',(3.5000008470667,-1.33997810357527,0.628091493562486));
#15778=CARTESIAN_POINT('Ctrl Pts',(3.50000049017339,-1.34160279315579,0.620357239364781));
#15779=CARTESIAN_POINT('Ctrl Pts',(3.50000026118253,-1.3426452308862,0.615394766232079));
#15780=CARTESIAN_POINT('Ctrl Pts',(3.5,-1.34331313055125,0.610351689051435));
#15781=CARTESIAN_POINT('Ctrl Pts',(3.5,-1.34358136363184,0.605270327458634));
#15782=CARTESIAN_POINT('',(3.5,0.723888888888889,0.7));
#15783=CARTESIAN_POINT('Ctrl Pts',(3.5,1.37552980833516,0.));
#15784=CARTESIAN_POINT('Ctrl Pts',(3.5,1.37020035376703,0.10097504527886));
#15785=CARTESIAN_POINT('Ctrl Pts',(3.5,1.36487063968137,0.201951358354439));
#15786=CARTESIAN_POINT('Ctrl Pts',(3.5,1.35422120417274,0.403707279015233));
#15787=CARTESIAN_POINT('Ctrl Pts',(3.5,1.34890134846466,0.504489444860456));
#15788=CARTESIAN_POINT('Ctrl Pts',(3.5,1.34358136363184,0.605270327458635));
#15789=CARTESIAN_POINT('Ctrl Pts',(3.50000000097418,-1.37552980835478,3.46944695195361E-18));
#15790=CARTESIAN_POINT('Ctrl Pts',(3.50374047168104,-1.36494504174376,0.201972406882836));
#15791=CARTESIAN_POINT('Ctrl Pts',(3.50748098869546,-1.35436027657305,0.403944812985359));
#15792=CARTESIAN_POINT('Ctrl Pts',(3.51122155284351,-1.34377551287676,0.605917218294091));
#15793=CARTESIAN_POINT('Ctrl Pts',(2.69119625874569,-1.35924722858667,-7.54309614812119E-5));
#15794=CARTESIAN_POINT('Ctrl Pts',(2.69653217397324,-1.34866266892899,0.20189683354744));
#15795=CARTESIAN_POINT('Ctrl Pts',(2.70186816749714,-1.3380781117335,0.403869096002786));
#15796=CARTESIAN_POINT('Ctrl Pts',(2.7072042346663,-1.32749355863083,0.605841357314298));
#15797=CARTESIAN_POINT('Ctrl Pts',(1.88267190563219,-1.32763345268679,-0.000212792412547521));
#15798=CARTESIAN_POINT('Ctrl Pts',(1.88960380459144,-1.31704931403188,0.201759213581099));
#15799=CARTESIAN_POINT('Ctrl Pts',(1.89653581411498,-1.30646518166523,0.403731216009517));
#15800=CARTESIAN_POINT('Ctrl Pts',(1.90346792975642,-1.29588105699583,0.605703215867581));
#15801=CARTESIAN_POINT('Ctrl Pts',(1.07441451989529,-1.27728918272486,-0.000429194541766893));
#15802=CARTESIAN_POINT('Ctrl Pts',(1.08294287068452,-1.26670581246828,0.201542410257184));
#15803=CARTESIAN_POINT('Ctrl Pts',(1.09147136321593,-1.25612245578053,0.403514009799157));
#15804=CARTESIAN_POINT('Ctrl Pts',(1.09999999999989,-1.24553911298205,0.605485603995245));
#15805=CARTESIAN_POINT('Ctrl Pts',(1.09999999916631,-1.24553911263844,0.605485603997431));
#15806=CARTESIAN_POINT('Ctrl Pts',(1.89930203168262,-1.29563783986497,0.605377360150118));
#15807=CARTESIAN_POINT('Ctrl Pts',(2.69958486793449,-1.32722445934619,0.605308375488923));
#15808=CARTESIAN_POINT('Ctrl Pts',(3.5,-1.34358136363184,0.605270327458634));
#15809=CARTESIAN_POINT('Ctrl Pts',(3.50204003610941,-1.24374118183538,0.7));
#15810=CARTESIAN_POINT('Ctrl Pts',(2.70080437300401,-1.2273695200909,0.7));
#15811=CARTESIAN_POINT('Ctrl Pts',(1.89984199608574,-1.1957170361627,0.7));
#15812=CARTESIAN_POINT('Ctrl Pts',(1.1,-1.14549341399196,0.7));
#15813=CARTESIAN_POINT('Ctrl Pts',(3.50144932661635,-1.27265074030048,0.7));
#15814=CARTESIAN_POINT('Ctrl Pts',(2.6998452019678,-1.25626413437997,0.699999727319846));
#15815=CARTESIAN_POINT('Ctrl Pts',(1.89847848223078,-1.22458382597074,0.70000077422621));
#15816=CARTESIAN_POINT('Ctrl Pts',(1.09819048660397,-1.17431102498992,0.7));
#15817=CARTESIAN_POINT('Ctrl Pts',(3.50042536655637,-1.322763754511,0.676632802377821));
#15818=CARTESIAN_POINT('Ctrl Pts',(2.69818680938114,-1.3063522351595,0.67664530655333));
#15819=CARTESIAN_POINT('Ctrl Pts',(1.89610976425884,-1.27462253270773,0.67666760713801));
#15820=CARTESIAN_POINT('Ctrl Pts',(1.09505363188407,-1.22426736091617,0.676703190608825));
#15821=CARTESIAN_POINT('Ctrl Pts',(3.50002334924346,-1.34243864233338,0.626926882269943));
#15822=CARTESIAN_POINT('Ctrl Pts',(2.6975332861013,-1.32603127467068,0.626959208652505));
#15823=CARTESIAN_POINT('Ctrl Pts',(1.89518106151152,-1.29430885982199,0.62701751976321));
#15824=CARTESIAN_POINT('Ctrl Pts',(1.09381704710221,-1.24396073223232,0.627109609335854));
#15825=CARTESIAN_POINT('Ctrl Pts',(3.5,-1.34358136363184,0.605270327458634));
#15826=CARTESIAN_POINT('Ctrl Pts',(2.69749615303,-1.32718177535833,0.605308474776761));
#15827=CARTESIAN_POINT('Ctrl Pts',(1.89512529323683,-1.29547288309274,0.605377720397184));
#15828=CARTESIAN_POINT('Ctrl Pts',(1.09374258853658,-1.24514653057163,0.605486452199395));
#15829=CARTESIAN_POINT('Ctrl Pts',(3.49999999991875,-1.24369946470729,0.7));
#15830=CARTESIAN_POINT('Ctrl Pts',(3.26917843083003,-1.23897560807887,0.7));
#15831=CARTESIAN_POINT('Ctrl Pts',(3.03837960179139,-1.23298334389983,0.7));
#15832=CARTESIAN_POINT('Ctrl Pts',(2.80762376541487,-1.22564400623233,0.7));
#15833=CARTESIAN_POINT('Ctrl Pts',(2.57739190516312,-1.2178709162388,0.7));
#15834=CARTESIAN_POINT('Ctrl Pts',(2.08463535466707,-1.20026407570248,0.7));
#15835=CARTESIAN_POINT('Ctrl Pts',(1.59210562457525,-1.17639367564078,0.7));
#15836=CARTESIAN_POINT('Ctrl Pts',(1.1,-1.14549341399196,0.7));
#15837=CARTESIAN_POINT('Origin',(5.4,-8.11656130105013E-18,0.7));
#15838=CARTESIAN_POINT('Ctrl Pts',(1.0744145198953,1.27728918272486,-0.000429194541767127));
#15839=CARTESIAN_POINT('Ctrl Pts',(1.08294287068452,1.26670581246828,0.201542410257184));
#15840=CARTESIAN_POINT('Ctrl Pts',(1.09147136321593,1.25612245578053,0.403514009799157));
#15841=CARTESIAN_POINT('Ctrl Pts',(1.0999999999999,1.24553911298205,0.605485603995245));
#15842=CARTESIAN_POINT('Ctrl Pts',(1.88267190563235,1.3276334526868,-0.000212792412547728));
#15843=CARTESIAN_POINT('Ctrl Pts',(1.8896038045916,1.31704931403189,0.201759213581098));
#15844=CARTESIAN_POINT('Ctrl Pts',(1.89653581411514,1.30646518166524,0.403731216009517));
#15845=CARTESIAN_POINT('Ctrl Pts',(1.90346792975658,1.29588105699584,0.605703215867581));
#15846=CARTESIAN_POINT('Ctrl Pts',(2.69119625874601,1.35924722858668,-7.54309614812134E-5));
#15847=CARTESIAN_POINT('Ctrl Pts',(2.69653217397356,1.348662668929,0.201896833547441));
#15848=CARTESIAN_POINT('Ctrl Pts',(2.70186816749745,1.33807811173351,0.403869096002786));
#15849=CARTESIAN_POINT('Ctrl Pts',(2.70720423466661,1.32749355863085,0.605841357314298));
#15850=CARTESIAN_POINT('Ctrl Pts',(3.50000000097466,1.37552980835479,-3.81639164714898E-17));
#15851=CARTESIAN_POINT('Ctrl Pts',(3.50374047168151,1.36494504174377,0.201972406882836));
#15852=CARTESIAN_POINT('Ctrl Pts',(3.50748098869594,1.35436027657306,0.403944812985359));
#15853=CARTESIAN_POINT('Ctrl Pts',(3.51122155284398,1.34377551287677,0.605917218294091));
#15854=CARTESIAN_POINT('Origin',(0.9,1.34328341716202,0.));
#15855=CARTESIAN_POINT('',(0.9,-1.23261418131727,0.605513513251856));
#15856=CARTESIAN_POINT('Ctrl Pts',(0.9,-1.23261418131727,0.605513513251856));
#15857=CARTESIAN_POINT('Ctrl Pts',(0.9,-1.23820195798151,0.504544236118289));
#15858=CARTESIAN_POINT('Ctrl Pts',(0.9,-1.24378834611607,0.403573587101897));
#15859=CARTESIAN_POINT('Ctrl Pts',(0.9,-1.25495246062481,0.201736610752668));
#15860=CARTESIAN_POINT('Ctrl Pts',(0.9,-1.26053033259331,0.100867703930409));
#15861=CARTESIAN_POINT('Ctrl Pts',(0.9,-1.266106713614,0.));
#15862=CARTESIAN_POINT('',(0.9,-1.13254484134404,0.7));
#15863=CARTESIAN_POINT('Ctrl Pts',(0.899999999937205,-1.13254484130906,
0.7));
#15864=CARTESIAN_POINT('Ctrl Pts',(0.899999996287105,-1.14047016437301,
0.699999998205918));
#15865=CARTESIAN_POINT('Ctrl Pts',(0.900001280561548,-1.14833327216777,
0.699006663725481));
#15866=CARTESIAN_POINT('Ctrl Pts',(0.900002371513522,-1.15599299513142,
0.697119896446058));
#15867=CARTESIAN_POINT('Ctrl Pts',(0.900002982478546,-1.16028266409831,
0.696063251566776));
#15868=CARTESIAN_POINT('Ctrl Pts',(0.900003528700818,-1.16450859688491,
0.694725368779139));
#15869=CARTESIAN_POINT('Ctrl Pts',(0.900003857331964,-1.16864431737637,
0.693116947675672));
#15870=CARTESIAN_POINT('Ctrl Pts',(0.900004447924614,-1.17607674172948,
0.690226407030055));
#15871=CARTESIAN_POINT('Ctrl Pts',(0.900004211500339,-1.18313828052408,
0.686496282267003));
#15872=CARTESIAN_POINT('Ctrl Pts',(0.900003280035406,-1.18968205680082,
0.682006679400108));
#15873=CARTESIAN_POINT('Ctrl Pts',(0.900002768383153,-1.19327654302499,
0.679540547464272));
#15874=CARTESIAN_POINT('Ctrl Pts',(0.900002064672634,-1.19671453445753,
0.676844382327844));
#15875=CARTESIAN_POINT('Ctrl Pts',(0.900001450170085,-1.19996775918788,
0.673925988054463));
#15876=CARTESIAN_POINT('Ctrl Pts',(0.900000850201302,-1.20314404102283,
0.67107661751105));
#15877=CARTESIAN_POINT('Ctrl Pts',(0.900000329673364,-1.20612495630093,
0.668032594545539));
#15878=CARTESIAN_POINT('Ctrl Pts',(0.900000346081477,-1.20888784276431,
0.664805176146368));
#15879=CARTESIAN_POINT('Ctrl Pts',(0.900000376514472,-1.21401231436848,
0.658819112599938));
#15880=CARTESIAN_POINT('Ctrl Pts',(0.900002057232535,-1.21838968018573,
0.652203523053766));
#15881=CARTESIAN_POINT('Ctrl Pts',(0.900002698394847,-1.22195969054856,
0.645123732731769));
#15882=CARTESIAN_POINT('Ctrl Pts',(0.900002763240662,-1.22232075393107,
0.644407697543824));
#15883=CARTESIAN_POINT('Ctrl Pts',(0.90000282009371,-1.22267351953901,0.643686895083047));
#15884=CARTESIAN_POINT('Ctrl Pts',(0.900002868017411,-1.22301789747605,
0.642961485862499));
#15885=CARTESIAN_POINT('Ctrl Pts',(0.900003341628975,-1.22642125256928,
0.635792544708285));
#15886=CARTESIAN_POINT('Ctrl Pts',(0.900002645022176,-1.22896979279554,
0.628258742918086));
#15887=CARTESIAN_POINT('Ctrl Pts',(0.900001532827652,-1.23061007098772,
0.6205286650049));
#15888=CARTESIAN_POINT('Ctrl Pts',(0.900000822323555,-1.23165793118585,
0.61559045329652));
#15889=CARTESIAN_POINT('Ctrl Pts',(0.900000000000001,-1.23233426661673,
0.610571479357261));
#15890=CARTESIAN_POINT('Ctrl Pts',(0.900000000000001,-1.23261418131727,
0.605513513251856));
#15891=CARTESIAN_POINT('',(0.9,1.13254484134404,0.7));
#15892=CARTESIAN_POINT('',(0.9,0.671641708581009,0.7));
#15893=CARTESIAN_POINT('',(0.9,1.23261418131727,0.605513513251856));
#15894=CARTESIAN_POINT('Ctrl Pts',(0.9,1.23261418131727,0.605513513251856));
#15895=CARTESIAN_POINT('Ctrl Pts',(0.9,1.23217633603244,0.613425232807268));
#15896=CARTESIAN_POINT('Ctrl Pts',(0.900001832787994,1.23077105609892,0.621244170085157));
#15897=CARTESIAN_POINT('Ctrl Pts',(0.900002580745575,1.22848219166492,0.628809599741497));
#15898=CARTESIAN_POINT('Ctrl Pts',(0.900002993068559,1.22722042035689,0.632980157827643));
#15899=CARTESIAN_POINT('Ctrl Pts',(0.90000314174678,1.22568915198244,0.637073706995481));
#15900=CARTESIAN_POINT('Ctrl Pts',(0.900002971484041,1.2238959908032,0.641061424759933));
#15901=CARTESIAN_POINT('Ctrl Pts',(0.900002662567364,1.22064256379503,0.648296551655426));
#15902=CARTESIAN_POINT('Ctrl Pts',(0.900001146653719,1.21656554418039,0.655104870690721));
#15903=CARTESIAN_POINT('Ctrl Pts',(0.900000540233788,1.21172928299109,0.66132323772617));
#15904=CARTESIAN_POINT('Ctrl Pts',(0.900000424918953,1.21080963534652,0.66250570210793));
#15905=CARTESIAN_POINT('Ctrl Pts',(0.900000351402035,1.20986240082127,0.663666762843393));
#15906=CARTESIAN_POINT('Ctrl Pts',(0.900000346234225,1.20888784277449,0.664805176146358));
#15907=CARTESIAN_POINT('Ctrl Pts',(0.900000336405833,1.20703438079614,0.666970266034709));
#15908=CARTESIAN_POINT('Ctrl Pts',(0.900000571869483,1.20508211779724,0.669053482241208));
#15909=CARTESIAN_POINT('Ctrl Pts',(0.900000903580486,1.20303784749416,0.671051418948595));
#15910=CARTESIAN_POINT('Ctrl Pts',(0.900001825932764,1.19735357006848,0.676606861644505));
#15911=CARTESIAN_POINT('Ctrl Pts',(0.900003332967427,1.19102482074992,0.681443262092019));
#15912=CARTESIAN_POINT('Ctrl Pts',(0.900003895332687,1.18421635668109,0.685507797106414));
#15913=CARTESIAN_POINT('Ctrl Pts',(0.900004254598985,1.17986677848026,0.688104419886002));
#15914=CARTESIAN_POINT('Ctrl Pts',(0.9000042929279,1.17532044218795,0.69038534615497));
#15915=CARTESIAN_POINT('Ctrl Pts',(0.900003997675654,1.17061445353731,0.692327416690341));
#15916=CARTESIAN_POINT('Ctrl Pts',(0.900003537640084,1.16328200409216,0.695353376818313));
#15917=CARTESIAN_POINT('Ctrl Pts',(0.900002259964378,1.15564663185935,0.697524398440697));
#15918=CARTESIAN_POINT('Ctrl Pts',(0.900001215101098,1.14785635641255,0.698771715080855));
#15919=CARTESIAN_POINT('Ctrl Pts',(0.900000537649455,1.14280542295857,0.699580430175527));
#15920=CARTESIAN_POINT('Ctrl Pts',(0.899999997568109,1.13768876957788,0.699999998835552));
#15921=CARTESIAN_POINT('Ctrl Pts',(0.899999999937205,1.13254484130906,0.7));
#15922=CARTESIAN_POINT('Ctrl Pts',(0.9,1.266106713614,0.));
#15923=CARTESIAN_POINT('Ctrl Pts',(0.9,1.26053025554556,0.100869097599589));
#15924=CARTESIAN_POINT('Ctrl Pts',(0.9,1.25495230648558,0.201739398169819));
#15925=CARTESIAN_POINT('Ctrl Pts',(0.9,1.24378819189631,0.403576374532447));
#15926=CARTESIAN_POINT('Ctrl Pts',(0.9,1.23820188085298,0.504545629805417));
#15927=CARTESIAN_POINT('Ctrl Pts',(0.9,1.23261418131727,0.605513513251856));
#15928=CARTESIAN_POINT('Ctrl Pts',(0.900000000000002,-1.266106713614,-8.15320033709099E-17));
#15929=CARTESIAN_POINT('Ctrl Pts',(0.908871090277923,-1.25552568177643,
0.201930159665972));
#15930=CARTESIAN_POINT('Ctrl Pts',(0.917742329685194,-1.24494466498547,
0.403860313587921));
#15931=CARTESIAN_POINT('Ctrl Pts',(0.926613720860141,-1.23436366359623,
0.605790461668883));
#15932=CARTESIAN_POINT('Ctrl Pts',(0.697441255022372,-1.25280938151844,
-5.71013218131409E-5));
#15933=CARTESIAN_POINT('Ctrl Pts',(0.706712389899261,-1.24222855501813,
0.201872952723963));
#15934=CARTESIAN_POINT('Ctrl Pts',(0.71598368260269,-1.23164774534186,0.403803000441224));
#15935=CARTESIAN_POINT('Ctrl Pts',(0.725255135891715,-1.22106695288555,
0.605733041729342));
#15936=CARTESIAN_POINT('Ctrl Pts',(0.494899146035781,-1.23832021354117,
-0.000119230777047918));
#15937=CARTESIAN_POINT('Ctrl Pts',(0.504570354086872,-1.2277396148863,0.201810708652083));
#15938=CARTESIAN_POINT('Ctrl Pts',(0.514241728780064,-1.21715903502506,
0.403740641123913));
#15939=CARTESIAN_POINT('Ctrl Pts',(0.523913273026478,-1.20657847439907,
0.605670566527588));
#15940=CARTESIAN_POINT('Ctrl Pts',(0.292373353339556,-1.22258574808743,
-0.000186633859775947));
#15941=CARTESIAN_POINT('Ctrl Pts',(0.302444661323169,-1.21200540195431,
0.201743181663441));
#15942=CARTESIAN_POINT('Ctrl Pts',(0.312516144861689,-1.20142507679253,
0.403672989556125));
#15943=CARTESIAN_POINT('Ctrl Pts',(0.322587807049886,-1.190844773096,0.605602789690272));
#15944=CARTESIAN_POINT('',(0.32407846024449,-1.19096124572524,0.605603291426262));
#15945=CARTESIAN_POINT('Ctrl Pts',(0.292382661757373,-1.22257596919059,
-1.26634813746307E-16));
#15946=CARTESIAN_POINT('Ctrl Pts',(0.302948004341657,-1.21203750712027,
0.201867748891544));
#15947=CARTESIAN_POINT('Ctrl Pts',(0.313513270922098,-1.20149926476964,
0.403735512620674));
#15948=CARTESIAN_POINT('Ctrl Pts',(0.324078460244491,-1.19096124572524,
0.605603291426262));
#15949=CARTESIAN_POINT('Ctrl Pts',(0.324078460244487,-1.19096124572524,
0.605603291426262));
#15950=CARTESIAN_POINT('Ctrl Pts',(0.515976798438381,-1.20595780001216,
0.605571001180369));
#15951=CARTESIAN_POINT('Ctrl Pts',(0.707956283694857,-1.21982772882273,
0.605541108414459));
#15952=CARTESIAN_POINT('Ctrl Pts',(0.900000000000001,-1.23261418131727,
0.605513513251856));
#15953=CARTESIAN_POINT('Ctrl Pts',(0.906632491847682,-1.13298681949577,
0.7));
#15954=CARTESIAN_POINT('Ctrl Pts',(0.714963137593258,-1.12022681655782,
0.7));
#15955=CARTESIAN_POINT('Ctrl Pts',(0.52336552158394,-1.10638609587519,0.7));
#15956=CARTESIAN_POINT('Ctrl Pts',(0.331856371369197,-1.09142177001972,
0.7));
#15957=CARTESIAN_POINT('Ctrl Pts',(0.904714827274509,-1.16179226195561,
0.7));
#15958=CARTESIAN_POINT('Ctrl Pts',(0.712937153454425,-1.14901967286075,
0.69999980360337));
#15959=CARTESIAN_POINT('Ctrl Pts',(0.521230340369869,-1.13516557394852,
0.700000229443053));
#15960=CARTESIAN_POINT('Ctrl Pts',(0.329608751265076,-1.12018616744754,
0.7));
#15961=CARTESIAN_POINT('Ctrl Pts',(0.901389714107723,-1.21173913866089,
0.676722045797292));
#15962=CARTESIAN_POINT('Ctrl Pts',(0.709425477581998,-1.19894546296063,
0.676731074746188));
#15963=CARTESIAN_POINT('Ctrl Pts',(0.517526696841433,-1.18506766126723,
0.67674067107047));
#15964=CARTESIAN_POINT('Ctrl Pts',(0.325711429829026,-1.17006296935233,
0.676751229163451));
#15965=CARTESIAN_POINT('Ctrl Pts',(0.900079298017777,-1.23142303740181,
0.627132481749528));
#15966=CARTESIAN_POINT('Ctrl Pts',(0.708040181852795,-1.21863106773591,
0.627155851652593));
#15967=CARTESIAN_POINT('Ctrl Pts',(0.516066269599777,-1.20475540724405,
0.627181012790208));
#15968=CARTESIAN_POINT('Ctrl Pts',(0.324172915772929,-1.18975243096407,
0.627208352638976));
#15969=CARTESIAN_POINT('Ctrl Pts',(0.900000000000001,-1.23261418131727,
0.605513513251856));
#15970=CARTESIAN_POINT('Ctrl Pts',(0.707956283694857,-1.21982772882273,
0.605541108414459));
#15971=CARTESIAN_POINT('Ctrl Pts',(0.515976798438381,-1.20595780001216,
0.605571001180369));
#15972=CARTESIAN_POINT('Ctrl Pts',(0.324078460244487,-1.19096124572524,
0.605603291426262));
#15973=CARTESIAN_POINT('',(0.3318563713692,-1.09142177001972,0.7));
#15974=CARTESIAN_POINT('Origin',(0.3318563713692,-1.09142177001972,0.6));
#15975=CARTESIAN_POINT('Ctrl Pts',(0.899999999937167,-1.13254484130906,
0.7));
#15976=CARTESIAN_POINT('Ctrl Pts',(0.710543123935439,-1.11990737114256,
0.7));
#15977=CARTESIAN_POINT('Ctrl Pts',(0.521156529292483,-1.10621348751457,
0.7));
#15978=CARTESIAN_POINT('Ctrl Pts',(0.331856371369197,-1.09142177001972,
0.7));
#15979=CARTESIAN_POINT('Origin',(5.4,-8.11656130105013E-18,0.7));
#15980=CARTESIAN_POINT('',(0.3318563713692,1.09142177001972,0.7));
#15981=CARTESIAN_POINT('',(0.3318563713692,-0.7,0.7));
#15982=CARTESIAN_POINT('Ctrl Pts',(0.3318563713692,1.09142177001972,0.7));
#15983=CARTESIAN_POINT('Ctrl Pts',(0.521156529292483,1.10621348751457,0.7));
#15984=CARTESIAN_POINT('Ctrl Pts',(0.710543123935438,1.11990737114256,0.7));
#15985=CARTESIAN_POINT('Ctrl Pts',(0.899999999937165,1.13254484130906,0.7));
#15986=CARTESIAN_POINT('Ctrl Pts',(0.292373353339556,1.22258574808743,-0.000186633859776018));
#15987=CARTESIAN_POINT('Ctrl Pts',(0.30244466132317,1.21200540195431,0.20174318166344));
#15988=CARTESIAN_POINT('Ctrl Pts',(0.31251614486169,1.20142507679253,0.403672989556124));
#15989=CARTESIAN_POINT('Ctrl Pts',(0.322587807049886,1.190844773096,0.605602789690271));
#15990=CARTESIAN_POINT('Ctrl Pts',(0.494899146035781,1.23832021354117,-0.000119230777047989));
#15991=CARTESIAN_POINT('Ctrl Pts',(0.504570354086872,1.2277396148863,0.201810708652083));
#15992=CARTESIAN_POINT('Ctrl Pts',(0.514241728780064,1.21715903502506,0.403740641123914));
#15993=CARTESIAN_POINT('Ctrl Pts',(0.523913273026478,1.20657847439907,0.605670566527587));
#15994=CARTESIAN_POINT('Ctrl Pts',(0.697441255022371,1.25280938151844,-5.71013218130602E-5));
#15995=CARTESIAN_POINT('Ctrl Pts',(0.70671238989926,1.24222855501813,0.201872952723963));
#15996=CARTESIAN_POINT('Ctrl Pts',(0.715983682602689,1.23164774534186,0.403803000441224));
#15997=CARTESIAN_POINT('Ctrl Pts',(0.725255135891714,1.22106695288555,0.605733041729342));
#15998=CARTESIAN_POINT('Ctrl Pts',(0.9,1.266106713614,1.73472347597681E-18));
#15999=CARTESIAN_POINT('Ctrl Pts',(0.908871090277921,1.25552568177643,0.201930159665973));
#16000=CARTESIAN_POINT('Ctrl Pts',(0.917742329685192,1.24494466498547,0.403860313587921));
#16001=CARTESIAN_POINT('Ctrl Pts',(0.92661372086014,1.23436366359623,0.605790461668883));
#16002=CARTESIAN_POINT('',(0.32407846024449,1.19096124572524,0.605603291426262));
#16003=CARTESIAN_POINT('Ctrl Pts',(0.9,1.23261418131727,0.605513513251856));
#16004=CARTESIAN_POINT('Ctrl Pts',(0.707956283694857,1.21982772882273,0.605541108414459));
#16005=CARTESIAN_POINT('Ctrl Pts',(0.515976798438382,1.20595780001216,0.60557100118037));
#16006=CARTESIAN_POINT('Ctrl Pts',(0.32407846024449,1.19096124572524,0.605603291426262));
#16007=CARTESIAN_POINT('Ctrl Pts',(0.324078460244491,1.19096124572524,0.605603291426262));
#16008=CARTESIAN_POINT('Ctrl Pts',(0.313513270922098,1.20149926476964,0.403735512620674));
#16009=CARTESIAN_POINT('Ctrl Pts',(0.302948004341658,1.21203750712026,0.201867748891544));
#16010=CARTESIAN_POINT('Ctrl Pts',(0.292382661757373,1.22257596919059,3.4477629085039E-17));
#16011=CARTESIAN_POINT('Ctrl Pts',(0.3318563713692,1.09142177001972,0.7));
#16012=CARTESIAN_POINT('Ctrl Pts',(0.523365521583941,1.10638609587519,0.7));
#16013=CARTESIAN_POINT('Ctrl Pts',(0.714963137593258,1.12022681655782,0.7));
#16014=CARTESIAN_POINT('Ctrl Pts',(0.906632491847681,1.13298681949577,0.7));
#16015=CARTESIAN_POINT('Ctrl Pts',(0.329608751265078,1.12018616744754,0.7));
#16016=CARTESIAN_POINT('Ctrl Pts',(0.52123034036987,1.13516557394852,0.700000229443053));
#16017=CARTESIAN_POINT('Ctrl Pts',(0.712937153454426,1.14901967286075,0.699999803603371));
#16018=CARTESIAN_POINT('Ctrl Pts',(0.904714827274509,1.16179226195561,0.700000000000001));
#16019=CARTESIAN_POINT('Ctrl Pts',(0.325711429829028,1.17006296935233,0.676751229163452));
#16020=CARTESIAN_POINT('Ctrl Pts',(0.517526696841433,1.18506766126723,0.67674067107047));
#16021=CARTESIAN_POINT('Ctrl Pts',(0.709425477581997,1.19894546296063,0.676731074746189));
#16022=CARTESIAN_POINT('Ctrl Pts',(0.901389714107722,1.21173913866089,0.676722045797292));
#16023=CARTESIAN_POINT('Ctrl Pts',(0.324172915772932,1.18975243096407,0.627208352638976));
#16024=CARTESIAN_POINT('Ctrl Pts',(0.516066269599778,1.20475540724405,0.627181012790208));
#16025=CARTESIAN_POINT('Ctrl Pts',(0.708040181852794,1.21863106773591,0.627155851652593));
#16026=CARTESIAN_POINT('Ctrl Pts',(0.900079298017776,1.23142303740181,0.627132481749528));
#16027=CARTESIAN_POINT('Ctrl Pts',(0.32407846024449,1.19096124572524,0.605603291426262));
#16028=CARTESIAN_POINT('Ctrl Pts',(0.515976798438382,1.20595780001216,0.60557100118037));
#16029=CARTESIAN_POINT('Ctrl Pts',(0.707956283694857,1.21982772882273,0.605541108414459));
#16030=CARTESIAN_POINT('Ctrl Pts',(0.9,1.23261418131727,0.605513513251856));
#16031=CARTESIAN_POINT('Origin',(0.331856371369202,1.09142177001972,0.6));
#16032=CARTESIAN_POINT('Origin',(0.331856371369202,1.09142177001972,0.6));
#16033=CARTESIAN_POINT('Origin',(0.331856371369201,1.09142177001972,0.6));
#16034=CARTESIAN_POINT('Origin',(0.331856371369202,1.09142177001972,0.6));
#16035=CARTESIAN_POINT('Origin',(10.4681436286308,1.08420482079361,0.6));
#16036=CARTESIAN_POINT('Origin',(10.4681436276939,1.08420482084454,0.6));
#16037=CARTESIAN_POINT('',(10.5680065821063,1.08420482079361,0.605233595624295));
#16038=CARTESIAN_POINT('Origin',(10.4681436286308,1.08420482079361,0.6));
#16039=CARTESIAN_POINT('Origin',(10.4681436286308,1.08420482079361,0.6));
#16040=CARTESIAN_POINT('Origin',(0.3318563713692,-1.09142177001972,0.6));
#16041=CARTESIAN_POINT('Origin',(0.331856371369201,-1.09142177001972,0.6));
#16042=CARTESIAN_POINT('Origin',(0.3318563713692,-1.09142177001972,0.6));
#16043=CARTESIAN_POINT('Origin',(0.3318563713692,-0.7,0.6));
#16044=CARTESIAN_POINT('Ctrl Pts',(0.2922895713475,-1.22266882276207,-0.00177864096060679));
#16045=CARTESIAN_POINT('Ctrl Pts',(0.302885944515497,-1.21209940820877,
0.200681988163859));
#16046=CARTESIAN_POINT('Ctrl Pts',(0.313482241236256,-1.20153021465708,
0.403142632212487));
#16047=CARTESIAN_POINT('Ctrl Pts',(0.324078460244491,-1.19096124572524,
0.605603291426262));
#16048=CARTESIAN_POINT('Ctrl Pts',(0.264022491930188,-1.22039553779506,
-0.000415890128406236));
#16049=CARTESIAN_POINT('Ctrl Pts',(0.274621881512248,-1.20982222712748,
0.202044379074236));
#16050=CARTESIAN_POINT('Ctrl Pts',(0.285221154833576,-1.19924944554801,
0.404504681968985));
#16051=CARTESIAN_POINT('Ctrl Pts',(0.29582042516239,-1.18867654001483,0.606964977361795));
#16052=CARTESIAN_POINT('Ctrl Pts',(0.216712469170969,-1.1940874043406,0.000690255297866666));
#16053=CARTESIAN_POINT('Ctrl Pts',(0.227319688237882,-1.18351239299796,
0.203150045648192));
#16054=CARTESIAN_POINT('Ctrl Pts',(0.237926932441998,-1.17293746916702,
0.405609838636422));
#16055=CARTESIAN_POINT('Ctrl Pts',(0.248534117816369,-1.1623628476683,0.608069650238703));
#16056=CARTESIAN_POINT('Ctrl Pts',(0.200219987929043,-1.14439035743082,
-0.00103956457010847));
#16057=CARTESIAN_POINT('Ctrl Pts',(0.210830491339948,-1.13382006821851,
0.201420337884579));
#16058=CARTESIAN_POINT('Ctrl Pts',(0.221440906577676,-1.12324995278282,
0.403880253819325));
#16059=CARTESIAN_POINT('Ctrl Pts',(0.232051411471599,-1.11268010558856,
0.606340179010355));
#16060=CARTESIAN_POINT('Ctrl Pts',(0.200161975173303,-1.12312592850316,
-0.00214651389202307));
#16061=CARTESIAN_POINT('Ctrl Pts',(0.210772455448684,-1.11255764422181,
0.200313510564959));
#16062=CARTESIAN_POINT('Ctrl Pts',(0.221382936352032,-1.1019895901204,0.402773547004277));
#16063=CARTESIAN_POINT('Ctrl Pts',(0.231993417893744,-1.09142177001972,
0.605233595624295));
#16064=CARTESIAN_POINT('Origin',(10.4681436286308,-1.08420482109828,0.6));
#16065=CARTESIAN_POINT('',(10.5680065821063,-1.08420482079361,0.605233595624295));
#16066=CARTESIAN_POINT('Origin',(10.4681436286308,-1.08420482099672,0.600000000000001));
#16067=CARTESIAN_POINT('Origin',(10.4681436286308,-1.08420482109828,0.6));
#16068=CARTESIAN_POINT('Origin',(10.4681436286308,0.7,0.6));
#16069=CARTESIAN_POINT('',(10.5680065821063,0.7,0.605233595624295));
#16070=CARTESIAN_POINT('Ctrl Pts',(10.599839982685,-1.11594741464673,-0.00218387205330164));
#16071=CARTESIAN_POINT('Ctrl Pts',(10.5892288496247,-1.10536637943871,0.200288608282177));
#16072=CARTESIAN_POINT('Ctrl Pts',(10.5786177161011,-1.0947855138519,0.402761097457634));
#16073=CARTESIAN_POINT('Ctrl Pts',(10.5680065821063,-1.08420482079362,0.605233595624295));
#16074=CARTESIAN_POINT('Ctrl Pts',(10.5997613205547,-1.14474784499259,-0.000682909193257743));
#16075=CARTESIAN_POINT('Ctrl Pts',(10.5891501209488,-1.13416481604349,0.201789447273867));
#16076=CARTESIAN_POINT('Ctrl Pts',(10.5785391399155,-1.12358205581644,0.404261829287571));
#16077=CARTESIAN_POINT('Ctrl Pts',(10.5679279386544,-1.11299934606825,0.606734202078189));
#16078=CARTESIAN_POINT('Ctrl Pts',(10.5764119435127,-1.19466846760808,0.000702210001053139));
#16079=CARTESIAN_POINT('Ctrl Pts',(10.5658041809617,-1.18408222297768,0.203174550667819));
#16080=CARTESIAN_POINT('Ctrl Pts',(10.5551963844732,-1.17349608774572,0.405646894856767));
#16081=CARTESIAN_POINT('Ctrl Pts',(10.544588659013,-1.16291012508165,0.608119251464957));
#16082=CARTESIAN_POINT('Ctrl Pts',(10.5269342003857,-1.21442651155969,-0.000858270497959616));
#16083=CARTESIAN_POINT('Ctrl Pts',(10.5163317654776,-1.20384274018949,0.201614467507756));
#16084=CARTESIAN_POINT('Ctrl Pts',(10.5057293269973,-1.1932591813998,0.404087216090532));
#16085=CARTESIAN_POINT('Ctrl Pts',(10.4951269905998,-1.18267571840064,0.606559974437339));
#16086=CARTESIAN_POINT('Ctrl Pts',(10.5053655128635,-1.21565094114741,-0.0019246498908503));
#16087=CARTESIAN_POINT('Ctrl Pts',(10.4947646468921,-1.20506932615592,0.200548282383137));
#16088=CARTESIAN_POINT('Ctrl Pts',(10.4841638390504,-1.19448787589602,0.403021225840181));
#16089=CARTESIAN_POINT('Ctrl Pts',(10.4735630903435,-1.18390659316268,0.605494180667945));
#16090=CARTESIAN_POINT('Ctrl Pts',(10.5997255308004,-1.11583328740478,1.02782365951626E-16));
#16091=CARTESIAN_POINT('Ctrl Pts',(10.589152548365,-1.10529029582828,0.201744523047832));
#16092=CARTESIAN_POINT('Ctrl Pts',(10.5785795654695,-1.09474747266587,0.40348905487273));
#16093=CARTESIAN_POINT('Ctrl Pts',(10.5680065821063,-1.08420482079362,0.605233595624295));
#16094=CARTESIAN_POINT('Ctrl Pts',(10.5053638082297,1.21564923960921,-0.0018920919656423));
#16095=CARTESIAN_POINT('Ctrl Pts',(10.4947635104759,1.20506819181477,0.200569987667808));
#16096=CARTESIAN_POINT('Ctrl Pts',(10.4841632708454,1.19448730873444,0.403032078483127));
#16097=CARTESIAN_POINT('Ctrl Pts',(10.4735630903435,1.18390659316268,0.605494180667945));
#16098=CARTESIAN_POINT('Ctrl Pts',(10.5341220579192,1.21401666636749,-0.000470252816738081));
#16099=CARTESIAN_POINT('Ctrl Pts',(10.5235196325477,1.20343268662274,0.201991562854702));
#16100=CARTESIAN_POINT('Ctrl Pts',(10.5129172908767,1.19284910679518,0.404453403808947));
#16101=CARTESIAN_POINT('Ctrl Pts',(10.5023149573519,1.18226542681329,0.606915239027137));
#16102=CARTESIAN_POINT('Ctrl Pts',(10.5827170203615,1.18801090922716,0.000717463067903341));
#16103=CARTESIAN_POINT('Ctrl Pts',(10.5721088691741,1.17742555398174,0.203178921531494));
#16104=CARTESIAN_POINT('Ctrl Pts',(10.5615007184277,1.16684027916303,0.405640383775807));
#16105=CARTESIAN_POINT('Ctrl Pts',(10.5508925935528,1.15625520969485,0.60810185787831));
#16106=CARTESIAN_POINT('Ctrl Pts',(10.5997792798033,1.13754603572512,-0.00102559206997387));
#16107=CARTESIAN_POINT('Ctrl Pts',(10.5891686973038,1.12696411138589,0.201435946515793));
#16108=CARTESIAN_POINT('Ctrl Pts',(10.5785581831385,1.11638231376635,0.40389749513889));
#16109=CARTESIAN_POINT('Ctrl Pts',(10.5679475995174,1.10580071474959,0.606359050464716));
#16110=CARTESIAN_POINT('Ctrl Pts',(10.5998382764002,1.11594571320176,-0.00215131420076595));
#16111=CARTESIAN_POINT('Ctrl Pts',(10.5892277121014,1.10536524516024,0.200310313518148));
#16112=CARTESIAN_POINT('Ctrl Pts',(10.5786171473394,1.09478494672192,0.402771950076102));
#16113=CARTESIAN_POINT('Ctrl Pts',(10.5680065821063,1.08420482079361,0.605233595624295));
#16114=CARTESIAN_POINT('Ctrl Pts',(10.5680065821063,1.08420482079361,0.605233595624295));
#16115=CARTESIAN_POINT('Ctrl Pts',(10.5785795654695,1.09474747266587,0.40348905487273));
#16116=CARTESIAN_POINT('Ctrl Pts',(10.589152548365,1.10529029582828,0.201744523047831));
#16117=CARTESIAN_POINT('Ctrl Pts',(10.5997255308004,1.11583328740478,1.07661275727811E-16));
#16118=CARTESIAN_POINT('Ctrl Pts',(10.1947388861048,1.09885088260187,0.7));
#16119=CARTESIAN_POINT('Ctrl Pts',(10.285877616441,1.09404209584202,0.7));
#16120=CARTESIAN_POINT('Ctrl Pts',(10.3770124662346,1.0891584122264,0.7));
#16121=CARTESIAN_POINT('Ctrl Pts',(10.4681436286308,1.08420482079361,0.7));
#16122=CARTESIAN_POINT('Ctrl Pts',(10.196260416419,1.12768774893097,0.700000000000001));
#16123=CARTESIAN_POINT('Ctrl Pts',(10.2874149314686,1.12287675076168,0.699999949550842));
#16124=CARTESIAN_POINT('Ctrl Pts',(10.3785648662465,1.11799094453753,0.700000051218742));
#16125=CARTESIAN_POINT('Ctrl Pts',(10.4697107510168,1.11303515260326,0.7));
#16126=CARTESIAN_POINT('Ctrl Pts',(10.1988975981852,1.17766904563614,0.67669140632491));
#16127=CARTESIAN_POINT('Ctrl Pts',(10.2900793016129,1.17285439035486,0.676693724638983));
#16128=CARTESIAN_POINT('Ctrl Pts',(10.3812557252598,1.16796482352885,0.676696026813929));
#16129=CARTESIAN_POINT('Ctrl Pts',(10.4724269697127,1.16300539549315,0.676698381019544));
#16130=CARTESIAN_POINT('Ctrl Pts',(10.1999375452555,1.19737868557977,0.627098033786781));
#16131=CARTESIAN_POINT('Ctrl Pts',(10.2911301919381,1.19256517083271,0.627104033151799));
#16132=CARTESIAN_POINT('Ctrl Pts',(10.382317043787,1.18767684023183,0.627110048826767));
#16133=CARTESIAN_POINT('Ctrl Pts',(10.4734985149421,1.18271860027509,0.627116141711795));
#16134=CARTESIAN_POINT('Ctrl Pts',(10.1999999975038,1.19856231440453,0.605472757505366));
#16135=CARTESIAN_POINT('Ctrl Pts',(10.2911933328565,1.19375025772558,0.605479840815741));
#16136=CARTESIAN_POINT('Ctrl Pts',(10.3823809652617,1.18886335120032,0.605486986548286));
#16137=CARTESIAN_POINT('Ctrl Pts',(10.4735630903435,1.18390659316268,0.605494180667944));
#16138=CARTESIAN_POINT('Ctrl Pts',(0.200159601751749,1.12312829248604,-0.00219180147311912));
#16139=CARTESIAN_POINT('Ctrl Pts',(0.210770873167554,1.11255922017607,0.200283318842441));
#16140=CARTESIAN_POINT('Ctrl Pts',(0.221382145211419,1.10199037808008,0.402758451142111));
#16141=CARTESIAN_POINT('Ctrl Pts',(0.231993417893744,1.09142177001972,0.605233595624295));
#16142=CARTESIAN_POINT('Ctrl Pts',(0.200236952094631,1.15148086499205,-0.000715869007730825));
#16143=CARTESIAN_POINT('Ctrl Pts',(0.210848310847714,1.14090905181173,0.201759082033021));
#16144=CARTESIAN_POINT('Ctrl Pts',(0.221459381762758,1.13033759660317,0.404234066901971));
#16145=CARTESIAN_POINT('Ctrl Pts',(0.232070742664217,1.11976621744484,0.606709040139042));
#16146=CARTESIAN_POINT('Ctrl Pts',(0.222806696702742,1.20067708175657,0.000669311976984441));
#16147=CARTESIAN_POINT('Ctrl Pts',(0.233413416075889,1.19010082554658,0.203144236955742));
#16148=CARTESIAN_POINT('Ctrl Pts',(0.244020198555212,1.17952469009474,0.405619164345205));
#16149=CARTESIAN_POINT('Ctrl Pts',(0.254626870458834,1.16894881850735,0.608094110943904));
#16150=CARTESIAN_POINT('Ctrl Pts',(0.271086891015657,1.22096622390789,-0.000801865493577694));
#16151=CARTESIAN_POINT('Ctrl Pts',(0.281686280594249,1.21039315447922,0.201673594461172));
#16152=CARTESIAN_POINT('Ctrl Pts',(0.292285672737775,1.1998203699977,0.404149068703718));
#16153=CARTESIAN_POINT('Ctrl Pts',(0.302884933932915,1.18924771644243,0.606624555877912));
#16154=CARTESIAN_POINT('Ctrl Pts',(0.292287201081515,1.22267118699778,-0.00182392867695869));
#16155=CARTESIAN_POINT('Ctrl Pts',(0.302884364349574,1.21210098433295,0.200651796350731));
#16156=CARTESIAN_POINT('Ctrl Pts',(0.313481451159089,1.20153100270242,0.403127536304793));
#16157=CARTESIAN_POINT('Ctrl Pts',(0.324078460244491,1.19096124572524,0.605603291426262));
#16158=CARTESIAN_POINT('Origin',(10.6002740930491,1.4,-0.0104671912485891));
#16159=CARTESIAN_POINT('Origin',(0.331856371369202,1.09142177001972,0.6));
#16160=CARTESIAN_POINT('',(0.3318563713692,1.09142177001972,0.9));
#16161=CARTESIAN_POINT('',(0.0322675109428288,1.09142177001972,0.615700786872883));
#16162=CARTESIAN_POINT('Origin',(0.3318563713692,1.09142177001972,0.6));
#16163=CARTESIAN_POINT('',(0.308522637995069,1.39004019713626,0.616809874278785));
#16164=CARTESIAN_POINT('Origin',(0.331856371369202,1.09142177001972,0.6));
#16165=CARTESIAN_POINT('Origin',(0.331856371369201,1.09142177001972,0.6));
#16166=CARTESIAN_POINT('Origin',(10.4681436286308,1.08420482079361,0.6));
#16167=CARTESIAN_POINT('',(10.4681436286308,1.08420482109828,0.9));
#16168=CARTESIAN_POINT('',(10.4844020137689,1.3833101379008,0.616482542003833));
#16169=CARTESIAN_POINT('Origin',(10.4681436258201,1.08420482094639,0.6));
#16170=CARTESIAN_POINT('',(10.7677324890572,1.08420482079361,0.615700786872884));
#16171=CARTESIAN_POINT('Origin',(10.4681436286308,1.08420482079361,0.6));
#16172=CARTESIAN_POINT('Origin',(10.4681436286308,1.08420482079362,0.6));
#16173=CARTESIAN_POINT('Origin',(0.3318563713692,-1.09142177001972,0.6));
#16174=CARTESIAN_POINT('',(0.3318563713692,-1.09142177001972,0.9));
#16175=CARTESIAN_POINT('',(0.308522637995069,-1.39004019713626,0.616809874278785));
#16176=CARTESIAN_POINT('Origin',(0.3318563713692,-1.09142177001972,0.6));
#16177=CARTESIAN_POINT('',(0.0322675109428289,-1.09142177001972,0.615700786872884));
#16178=CARTESIAN_POINT('Origin',(0.3318563713692,-1.09142177001972,0.6));
#16179=CARTESIAN_POINT('Origin',(0.331856371369201,-1.09142177001972,0.6));
#16180=CARTESIAN_POINT('Origin',(0.3318563713692,-0.7,0.6));
#16181=CARTESIAN_POINT('',(0.0322675109428288,-0.7,0.615700786872883));
#16182=CARTESIAN_POINT('',(0.3318563713692,-0.7,0.9));
#16183=CARTESIAN_POINT('Ctrl Pts',(0.276048389810261,-1.42252533450788,
-0.00533608639730399));
#16184=CARTESIAN_POINT('Ctrl Pts',(0.28687338241706,-1.4116967417008,0.202045878554724));
#16185=CARTESIAN_POINT('Ctrl Pts',(0.297698133178874,-1.40086836142621,
0.409427865329919));
#16186=CARTESIAN_POINT('Ctrl Pts',(0.308522637995069,-1.39004019713626,
0.616809874278785));
#16187=CARTESIAN_POINT('Ctrl Pts',(0.191246496057484,-1.41570630783033,
-0.00124775669238285));
#16188=CARTESIAN_POINT('Ctrl Pts',(0.202080757839133,-1.40486573978029,
0.206133102090467));
#16189=CARTESIAN_POINT('Ctrl Pts',(0.212914648880055,-1.39402634701096,
0.413514041581016));
#16190=CARTESIAN_POINT('Ctrl Pts',(0.223748532748767,-1.38318608000504,
0.620894932085382));
#16191=CARTESIAN_POINT('Ctrl Pts',(0.0492682973509243,-1.33685850703924,
0.00207719607616587));
#16192=CARTESIAN_POINT('Ctrl Pts',(0.0601266125734448,-1.32601270457081,
0.209456583216085));
#16193=CARTESIAN_POINT('Ctrl Pts',(0.0709850253737815,-1.3151666447344,
0.416835949794532));
#16194=CARTESIAN_POINT('Ctrl Pts',(0.0818432319483421,-1.30432109509162,
0.624215353109623));
#16195=CARTESIAN_POINT('Ctrl Pts',(-0.000163444061205068,-1.18769013309795,
-0.00311869847265479));
#16196=CARTESIAN_POINT('Ctrl Pts',(0.0107049555364969,-1.17685886333949,
0.204261034729081));
#16197=CARTESIAN_POINT('Ctrl Pts',(0.0215730900970294,-1.16602762920277,
0.411640782964944));
#16198=CARTESIAN_POINT('Ctrl Pts',(0.0324414916763936,-1.15519677672624,
0.619020537031064));
#16199=CARTESIAN_POINT('Ctrl Pts',(-0.00033748371827097,-1.12389640457412,
-0.0064395729582146));
#16200=CARTESIAN_POINT('Ctrl Pts',(0.0105308471731094,-1.11307128361434,
0.200940534347673));
#16201=CARTESIAN_POINT('Ctrl Pts',(0.0213991787230862,-1.10224640406117,
0.408320654220332));
#16202=CARTESIAN_POINT('Ctrl Pts',(0.0322675109428289,-1.09142177001972,
0.615700786872884));
#16203=CARTESIAN_POINT('Ctrl Pts',(0.27632692456468,-1.42224670711126,5.13911829758129E-17));
#16204=CARTESIAN_POINT('Ctrl Pts',(0.287059068122268,-1.41151099373342,
0.20560326985903));
#16205=CARTESIAN_POINT('Ctrl Pts',(0.297790973931072,-1.40077548928706,
0.411206561171438));
#16206=CARTESIAN_POINT('Ctrl Pts',(0.308522637995069,-1.39004019713626,
0.616809874278785));
#16207=CARTESIAN_POINT('Ctrl Pts',(0.0322675109428289,-1.09142177001972,
0.615700786872884));
#16208=CARTESIAN_POINT('Ctrl Pts',(0.0215116733095221,-1.10213436178043,
0.410467178800746));
#16209=CARTESIAN_POINT('Ctrl Pts',(0.0107558363321879,-1.11284719399673,
0.205233583245308));
#16210=CARTESIAN_POINT('Ctrl Pts',(1.76901136968166E-16,-1.12356026268968,
-7.45931094670027E-17));
#16211=CARTESIAN_POINT('Origin',(10.4681436286308,-1.08420482109828,0.6));
#16212=CARTESIAN_POINT('',(10.7677324890572,-1.08420482079361,0.615700786872884));
#16213=CARTESIAN_POINT('',(10.4844020137689,-1.3833101379008,0.616482542003833));
#16214=CARTESIAN_POINT('Origin',(10.4681436286308,-1.08420482079361,0.600000000000001));
#16215=CARTESIAN_POINT('',(10.4681436258201,-1.08420482094639,0.9));
#16216=CARTESIAN_POINT('Origin',(10.4681436286308,-1.08420482109828,0.6));
#16217=CARTESIAN_POINT('Origin',(10.4681436286308,-1.08420482079361,0.6));
#16218=CARTESIAN_POINT('Origin',(10.4681436286308,0.7,0.6));
#16219=CARTESIAN_POINT('',(10.7677324890572,0.7,0.615700786872884));
#16220=CARTESIAN_POINT('',(10.4681436286308,0.7,0.9));
#16221=CARTESIAN_POINT('Ctrl Pts',(10.4681436286308,-1.08420482079361,0.9));
#16222=CARTESIAN_POINT('Ctrl Pts',(9.02115959826777,-1.16285813221549,0.9));
#16223=CARTESIAN_POINT('Ctrl Pts',(5.64262097844114,-1.30550334054488,0.9));
#16224=CARTESIAN_POINT('Ctrl Pts',(2.25816172369615,-1.24194126716656,0.9));
#16225=CARTESIAN_POINT('Ctrl Pts',(0.331856371369198,-1.09142177001972,
0.9));
#16226=CARTESIAN_POINT('Ctrl Pts',(10.4728449957889,-1.17069581622255,0.9));
#16227=CARTESIAN_POINT('Ctrl Pts',(9.02515960257209,-1.24945398332951,0.900002463983243));
#16228=CARTESIAN_POINT('Ctrl Pts',(5.64406008560805,-1.39235654229312,0.899995181674544));
#16229=CARTESIAN_POINT('Ctrl Pts',(2.25481214769604,-1.3286896492945,0.900006992415263));
#16230=CARTESIAN_POINT('Ctrl Pts',(0.325113511056834,-1.17771496230318,
0.9));
#16231=CARTESIAN_POINT('Ctrl Pts',(10.4809942371438,-1.32061731204901,0.830050158657121));
#16232=CARTESIAN_POINT('Ctrl Pts',(9.03210079995546,-1.3995487214628,0.829938185878055));
#16233=CARTESIAN_POINT('Ctrl Pts',(5.64656962219688,-1.54290142969263,0.82970437227026));
#16234=CARTESIAN_POINT('Ctrl Pts',(2.24896854757963,-1.47903552984056,0.829838703712927));
#16235=CARTESIAN_POINT('Ctrl Pts',(0.313425270489114,-1.32729771265557,
0.830156825336737));
#16236=CARTESIAN_POINT('Ctrl Pts',(10.4842082875648,-1.37974615923803,0.681348425135383));
#16237=CARTESIAN_POINT('Ctrl Pts',(9.03482793853036,-1.45862084618981,0.681058092399338));
#16238=CARTESIAN_POINT('Ctrl Pts',(5.64753778607331,-1.60187726023264,0.68045297450285));
#16239=CARTESIAN_POINT('Ctrl Pts',(2.24670449952385,-1.53809938127555,0.680799765935021));
#16240=CARTESIAN_POINT('Ctrl Pts',(0.308806004580392,-1.38641375285276,
0.681625057916928));
#16241=CARTESIAN_POINT('Ctrl Pts',(10.4844020137689,-1.3833101379008,0.616482542003833));
#16242=CARTESIAN_POINT('Ctrl Pts',(9.03499042108131,-1.46211428773623,0.616139856494792));
#16243=CARTESIAN_POINT('Ctrl Pts',(5.64759185703765,-1.60522711936681,0.615422163720642));
#16244=CARTESIAN_POINT('Ctrl Pts',(2.24657199659733,-1.54153220865049,0.615835494619844));
#16245=CARTESIAN_POINT('Ctrl Pts',(0.308522637995066,-1.39004019713626,
0.616809874278785));
#16246=CARTESIAN_POINT('Ctrl Pts',(0.308522637995066,-1.39004019713626,
0.616809874278785));
#16247=CARTESIAN_POINT('Ctrl Pts',(2.24657199659733,-1.54153220865049,0.615835494619844));
#16248=CARTESIAN_POINT('Ctrl Pts',(5.64759185703765,-1.60522711936681,0.615422163720642));
#16249=CARTESIAN_POINT('Ctrl Pts',(9.03499042108131,-1.46211428773623,0.616139856494792));
#16250=CARTESIAN_POINT('Ctrl Pts',(10.4844020137689,-1.3833101379008,0.616482542003833));
#16251=CARTESIAN_POINT('Ctrl Pts',(10.4681436258201,-1.08420482094639,0.900000000000001));
#16252=CARTESIAN_POINT('Ctrl Pts',(9.02115959639274,-1.16285813229465,0.9));
#16253=CARTESIAN_POINT('Ctrl Pts',(5.64262097750198,-1.30550334052724,0.9));
#16254=CARTESIAN_POINT('Ctrl Pts',(2.25816172369615,-1.24194126716656,0.9));
#16255=CARTESIAN_POINT('Ctrl Pts',(0.331856371369198,-1.09142177001972,
0.9));
#16256=CARTESIAN_POINT('Ctrl Pts',(10.8003433549902,-1.11672267507076,-0.00655160349952438));
#16257=CARTESIAN_POINT('Ctrl Pts',(10.7894730668347,-1.10588321133639,0.200865850630566));
#16258=CARTESIAN_POINT('Ctrl Pts',(10.7786027781932,-1.09504392553578,0.408283314033857));
#16259=CARTESIAN_POINT('Ctrl Pts',(10.7677324890572,-1.08420482079361,0.615700786872885));
#16260=CARTESIAN_POINT('Ctrl Pts',(10.8001073672393,-1.20312439623403,-0.00204868896805508));
#16261=CARTESIAN_POINT('Ctrl Pts',(10.7892368724076,-1.19227880391739,0.205368384315645));
#16262=CARTESIAN_POINT('Ctrl Pts',(10.7783670568079,-1.18143370221047,0.41278551899075));
#16263=CARTESIAN_POINT('Ctrl Pts',(10.7674965587017,-1.17058839661753,0.620202606234566));
#16264=CARTESIAN_POINT('Ctrl Pts',(10.7300137544668,-1.35289768637741,0.00210488808650419));
#16265=CARTESIAN_POINT('Ctrl Pts',(10.7191538066016,-1.34204221082848,0.209521911971666));
#16266=CARTESIAN_POINT('Ctrl Pts',(10.7082938463195,-1.33118673671862,0.416938933985702));
#16267=CARTESIAN_POINT('Ctrl Pts',(10.6974340169938,-1.32033143065575,0.624355970618915));
#16268=CARTESIAN_POINT('Ctrl Pts',(10.5816241002662,-1.4121605627967,-0.00257485550010117));
#16269=CARTESIAN_POINT('Ctrl Pts',(10.5707805459565,-1.4013126969686,0.204843391064434));
#16270=CARTESIAN_POINT('Ctrl Pts',(10.5599369567012,-1.39046512672587,0.412261650129749));
#16271=CARTESIAN_POINT('Ctrl Pts',(10.5490937145378,-1.37961751361469,0.619679923312015));
#16272=CARTESIAN_POINT('Ctrl Pts',(10.5169176890673,-1.41583338198674,-0.00577403633861717));
#16273=CARTESIAN_POINT('Ctrl Pts',(10.5060789456421,-1.40499213715574,0.201644806368331));
#16274=CARTESIAN_POINT('Ctrl Pts',(10.4952403861233,-1.39415105487295,0.40906366572247));
#16275=CARTESIAN_POINT('Ctrl Pts',(10.4844020137689,-1.3833101379008,0.616482542003833));
#16276=CARTESIAN_POINT('Ctrl Pts',(10.8,-1.11638029377732,-2.51534904016637E-17));
#16277=CARTESIAN_POINT('Ctrl Pts',(10.7892441634977,-1.10565496086826,0.205233586491178));
#16278=CARTESIAN_POINT('Ctrl Pts',(10.7784883265195,-1.09492980219801,0.410467182062988));
#16279=CARTESIAN_POINT('Ctrl Pts',(10.7677324890572,-1.08420482079361,0.615700786872885));
#16280=CARTESIAN_POINT('Ctrl Pts',(10.4844020137689,-1.3833101379008,0.616482542003833));
#16281=CARTESIAN_POINT('Ctrl Pts',(10.4951398148107,-1.39405045994841,0.410988344812119));
#16282=CARTESIAN_POINT('Ctrl Pts',(10.5058777995597,-1.40479094425298,0.205494164234945));
#16283=CARTESIAN_POINT('Ctrl Pts',(10.5166159648474,-1.4155315881283,-2.5652223401007E-16));
#16284=CARTESIAN_POINT('Ctrl Pts',(10.5169125872774,1.41582827901939,-0.0056764044152427));
#16285=CARTESIAN_POINT('Ctrl Pts',(10.5060755445066,1.40498873522851,0.20170989432247));
#16286=CARTESIAN_POINT('Ctrl Pts',(10.4952386855848,1.39414935393528,0.409096209702196));
#16287=CARTESIAN_POINT('Ctrl Pts',(10.4844020137689,1.3833101379008,0.616482542003833));
#16288=CARTESIAN_POINT('Ctrl Pts',(10.6031877991504,1.41093118264609,-0.00141083033817288));
#16289=CARTESIAN_POINT('Ctrl Pts',(10.5923442181457,1.40008262840665,0.205974657203891));
#16290=CARTESIAN_POINT('Ctrl Pts',(10.5815009048179,1.38923496752292,0.413360205434192));
#16291=CARTESIAN_POINT('Ctrl Pts',(10.5706576147941,1.37838663885266,0.62074571708141));
#16292=CARTESIAN_POINT('Ctrl Pts',(10.7489822201969,1.33286898269122,0.00215046584238339));
#16293=CARTESIAN_POINT('Ctrl Pts',(10.7381210493968,1.32201618867047,0.209534855263179));
#16294=CARTESIAN_POINT('Ctrl Pts',(10.7272598662103,1.31116338896628,0.416919242515175));
#16295=CARTESIAN_POINT('Ctrl Pts',(10.716398780155,1.30031077634578,0.624303643734563));
#16296=CARTESIAN_POINT('Ctrl Pts',(10.8001612475457,1.18151886169146,-0.00307678645922502));
#16297=CARTESIAN_POINT('Ctrl Pts',(10.7892926103682,1.17067663552019,0.20430785074418));
#16298=CARTESIAN_POINT('Ctrl Pts',(10.7784241800195,1.15983442267521,0.41169249890798));
#16299=CARTESIAN_POINT('Ctrl Pts',(10.7675555412906,1.14899250266155,0.619077151394146));
#16300=CARTESIAN_POINT('Ctrl Pts',(10.8003382383521,1.11671757294177,-0.00645397222975308));
#16301=CARTESIAN_POINT('Ctrl Pts',(10.7894696557425,1.1058798099729,0.200930938146656));
#16302=CARTESIAN_POINT('Ctrl Pts',(10.778601072647,1.09504222488243,0.408315857793383));
#16303=CARTESIAN_POINT('Ctrl Pts',(10.7677324890572,1.08420482079361,0.615700786872884));
#16304=CARTESIAN_POINT('Ctrl Pts',(10.5166159648474,1.4155315881283,3.37837396946483E-16));
#16305=CARTESIAN_POINT('Ctrl Pts',(10.5058777995597,1.40479094425298,0.205494164234944));
#16306=CARTESIAN_POINT('Ctrl Pts',(10.4951398148107,1.39405045994841,0.41098834481212));
#16307=CARTESIAN_POINT('Ctrl Pts',(10.4844020137689,1.3833101379008,0.616482542003833));
#16308=CARTESIAN_POINT('Ctrl Pts',(10.7677324890572,1.08420482079361,0.615700786872884));
#16309=CARTESIAN_POINT('Ctrl Pts',(10.7784883265195,1.09492980219801,0.410467182062988));
#16310=CARTESIAN_POINT('Ctrl Pts',(10.7892441634977,1.10565496086826,0.205233586491177));
#16311=CARTESIAN_POINT('Ctrl Pts',(10.8,1.11638029377732,-4.7271214720368E-17));
#16312=CARTESIAN_POINT('Ctrl Pts',(0.3318563713692,1.09142177001972,0.9));
#16313=CARTESIAN_POINT('Ctrl Pts',(1.77658538561441,1.20431139287985,0.9));
#16314=CARTESIAN_POINT('Ctrl Pts',(5.15852145577913,1.31798734362749,0.900000000000001));
#16315=CARTESIAN_POINT('Ctrl Pts',(8.53883158814675,1.18907590268945,0.9));
#16316=CARTESIAN_POINT('Ctrl Pts',(10.4681436286308,1.08420482079361,0.9));
#16317=CARTESIAN_POINT('Ctrl Pts',(0.325113511056836,1.17771496230318,0.9));
#16318=CARTESIAN_POINT('Ctrl Pts',(1.77238748853623,1.29094597754667,0.900005244311447));
#16319=CARTESIAN_POINT('Ctrl Pts',(5.15940689953628,1.40489117512763,0.899995532233175));
#16320=CARTESIAN_POINT('Ctrl Pts',(8.54259780483314,1.2757067056985,0.90000328531099));
#16321=CARTESIAN_POINT('Ctrl Pts',(10.4728449957889,1.17069581622255,0.9));
#16322=CARTESIAN_POINT('Ctrl Pts',(0.313425270489116,1.32729771265557,0.830156825336737));
#16323=CARTESIAN_POINT('Ctrl Pts',(1.76508272830699,1.44110107554431,0.829918234118879));
#16324=CARTESIAN_POINT('Ctrl Pts',(5.16095094050242,1.55552201031752,0.829677185710002));
#16325=CARTESIAN_POINT('Ctrl Pts',(8.54913632089268,1.4258591912674,0.829900861618366));
#16326=CARTESIAN_POINT('Ctrl Pts',(10.4809942371438,1.32061731204901,0.830050158657121));
#16327=CARTESIAN_POINT('Ctrl Pts',(0.308806004580394,1.38641375285276,0.681625057916928));
#16328=CARTESIAN_POINT('Ctrl Pts',(1.76222987578798,1.50017797416985,0.681006088930498));
#16329=CARTESIAN_POINT('Ctrl Pts',(5.16154986224672,1.61450132085358,0.68038246417749));
#16330=CARTESIAN_POINT('Ctrl Pts',(8.55170115551887,1.48491240850707,0.680961314820656));
#16331=CARTESIAN_POINT('Ctrl Pts',(10.4842082875648,1.37974615923803,0.681348425135383));
#16332=CARTESIAN_POINT('Ctrl Pts',(0.308522637995068,1.39004019713626,0.616809874278785));
#16333=CARTESIAN_POINT('Ctrl Pts',(1.76205965694675,1.50365920577193,0.616079089534579));
#16334=CARTESIAN_POINT('Ctrl Pts',(5.16158497046229,1.61783515152865,0.615338844765104));
#16335=CARTESIAN_POINT('Ctrl Pts',(8.55185322351876,1.48838233768137,0.616025627991778));
#16336=CARTESIAN_POINT('Ctrl Pts',(10.4844020137689,1.3833101379008,0.616482542003833));
#16337=CARTESIAN_POINT('Ctrl Pts',(10.4844020137689,1.3833101379008,0.616482542003833));
#16338=CARTESIAN_POINT('Ctrl Pts',(8.55185322351876,1.48838233768137,0.616025627991778));
#16339=CARTESIAN_POINT('Ctrl Pts',(5.16158497046229,1.61783515152865,0.615338844765104));
#16340=CARTESIAN_POINT('Ctrl Pts',(1.76205965694675,1.50365920577193,0.616079089534579));
#16341=CARTESIAN_POINT('Ctrl Pts',(0.308522637995068,1.39004019713626,0.616809874278785));
#16342=CARTESIAN_POINT('Ctrl Pts',(0.3318563713692,1.09142177001972,0.9));
#16343=CARTESIAN_POINT('Ctrl Pts',(1.77658538561441,1.20431139287985,0.9));
#16344=CARTESIAN_POINT('Ctrl Pts',(5.15852145577913,1.31798734362749,0.900000000000001));
#16345=CARTESIAN_POINT('Ctrl Pts',(8.53883158814675,1.18907590268945,0.9));
#16346=CARTESIAN_POINT('Ctrl Pts',(10.4681436286308,1.08420482079361,0.9));
#16347=CARTESIAN_POINT('Ctrl Pts',(-0.000344602063817145,1.12390349461883,
-0.00657539908256866));
#16348=CARTESIAN_POINT('Ctrl Pts',(0.0105261016091243,1.11307601020539,
0.200849983592616));
#16349=CARTESIAN_POINT('Ctrl Pts',(0.0213968059409475,1.10224876730309,
0.408275378840013));
#16350=CARTESIAN_POINT('Ctrl Pts',(0.0322675109428289,1.09142177001972,
0.615700786872884));
#16351=CARTESIAN_POINT('Ctrl Pts',(-0.000112549170678945,1.2089618047365,
-0.00214756610981592));
#16352=CARTESIAN_POINT('Ctrl Pts',(0.0107584275574203,1.19812589474889,
0.205277296000037));
#16353=CARTESIAN_POINT('Ctrl Pts',(0.021628504370896,1.18729063034778,0.412702239156743));
#16354=CARTESIAN_POINT('Ctrl Pts',(0.0324994852542487,1.17645511229507,
0.620127120417125));
#16355=CARTESIAN_POINT('Ctrl Pts',(0.0675181008536004,1.35659180908255,
0.00201426213057289));
#16356=CARTESIAN_POINT('Ctrl Pts',(0.0783748317004002,1.34574224493831,
0.20943904356877));
#16357=CARTESIAN_POINT('Ctrl Pts',(0.0892318011706237,1.33489254525337,
0.416863803530356));
#16358=CARTESIAN_POINT('Ctrl Pts',(0.100088380073201,1.32404321751407,0.624288602298589));
#16359=CARTESIAN_POINT('Ctrl Pts',(0.212439875011655,1.41741816253371,-0.00240566592686199));
#16360=CARTESIAN_POINT('Ctrl Pts',(0.223274062163905,1.40657840226088,0.20502076110302));
#16361=CARTESIAN_POINT('Ctrl Pts',(0.234108278795672,1.39573903465802,0.412447205628077));
#16362=CARTESIAN_POINT('Ctrl Pts',(0.244942059060342,1.38489960928785,0.619873667633733));
#16363=CARTESIAN_POINT('Ctrl Pts',(0.276041299849618,1.42253242682652,-0.00547191373834488));
#16364=CARTESIAN_POINT('Ctrl Pts',(0.286868655882245,1.41170146982041,0.201955326984501));
#16365=CARTESIAN_POINT('Ctrl Pts',(0.297695769965166,1.40087072543886,0.409382589539965));
#16366=CARTESIAN_POINT('Ctrl Pts',(0.308522637995069,1.39004019713626,0.616809874278785));
#16367=CARTESIAN_POINT('Ctrl Pts',(2.26869304592592E-17,1.12356026268968,
-3.16587034365767E-17));
#16368=CARTESIAN_POINT('Ctrl Pts',(0.0107558363321878,1.11284719399672,
0.205233583245308));
#16369=CARTESIAN_POINT('Ctrl Pts',(0.0215116733095221,1.10213436178043,
0.410467178800746));
#16370=CARTESIAN_POINT('Ctrl Pts',(0.0322675109428289,1.09142177001972,
0.615700786872884));
#16371=CARTESIAN_POINT('Ctrl Pts',(0.308522637995069,1.39004019713626,0.616809874278785));
#16372=CARTESIAN_POINT('Ctrl Pts',(0.297790973931072,1.40077548928706,0.411206561171438));
#16373=CARTESIAN_POINT('Ctrl Pts',(0.287059068122271,1.41151099373341,0.205603269859031));
#16374=CARTESIAN_POINT('Ctrl Pts',(0.276326924564681,1.42224670711126,-2.68882138776405E-16));
#16375=CARTESIAN_POINT('Ctrl Pts',(10.5166159648474,-1.4155315881283,0.));
#16376=CARTESIAN_POINT('Ctrl Pts',(10.5064062201588,-1.40475637621136,0.205603291426271));
#16377=CARTESIAN_POINT('Ctrl Pts',(10.4961964754701,-1.39398116429443,0.411206582852543));
#16378=CARTESIAN_POINT('Ctrl Pts',(10.4859867307814,-1.38320595237749,0.616809874278814));
#16379=CARTESIAN_POINT('Ctrl Pts',(7.10318628475318,-1.599994843061,0.));
#16380=CARTESIAN_POINT('Ctrl Pts',(7.09978773046573,-1.58921963114407,0.205603291426271));
#16381=CARTESIAN_POINT('Ctrl Pts',(7.09638917617828,-1.57844441922713,0.411206582852543));
#16382=CARTESIAN_POINT('Ctrl Pts',(7.09299062189083,-1.5676692073102,0.616809874278814));
#16383=CARTESIAN_POINT('Ctrl Pts',(3.68975660465893,-1.68747752195839,0.));
#16384=CARTESIAN_POINT('Ctrl Pts',(3.69316924077269,-1.67670231004145,0.205603291426272));
#16385=CARTESIAN_POINT('Ctrl Pts',(3.69658187688646,-1.66592709812452,0.411206582852543));
#16386=CARTESIAN_POINT('Ctrl Pts',(3.69999451300023,-1.65515188620758,0.616809874278814));
#16387=CARTESIAN_POINT('Ctrl Pts',(0.276326924564679,-1.42224670711126,
0.));
#16388=CARTESIAN_POINT('Ctrl Pts',(0.286550751079662,-1.41147149519433,
0.205603291426271));
#16389=CARTESIAN_POINT('Ctrl Pts',(0.296774577594646,-1.40069628327739,
0.411206582852543));
#16390=CARTESIAN_POINT('Ctrl Pts',(0.306998404109629,-1.38992107136046,
0.616809874278814));
#16391=CARTESIAN_POINT('Origin',(0.,-1.4,0.));
#16392=CARTESIAN_POINT('Origin',(5.4,-8.13935059369636E-18,0.9));
#16393=CARTESIAN_POINT('Ctrl Pts',(0.276326924564679,1.42224670711126,0.));
#16394=CARTESIAN_POINT('Ctrl Pts',(0.286550751079662,1.41147149519433,0.205603291426271));
#16395=CARTESIAN_POINT('Ctrl Pts',(0.296774577594645,1.40069628327739,0.411206582852543));
#16396=CARTESIAN_POINT('Ctrl Pts',(0.306998404109628,1.38992107136046,0.616809874278814));
#16397=CARTESIAN_POINT('Ctrl Pts',(3.68975660465893,1.68747752195839,0.));
#16398=CARTESIAN_POINT('Ctrl Pts',(3.6931692407727,1.67670231004145,0.205603291426271));
#16399=CARTESIAN_POINT('Ctrl Pts',(3.69658187688646,1.66592709812452,0.411206582852543));
#16400=CARTESIAN_POINT('Ctrl Pts',(3.69999451300023,1.65515188620758,0.616809874278814));
#16401=CARTESIAN_POINT('Ctrl Pts',(7.10318628475318,1.599994843061,0.));
#16402=CARTESIAN_POINT('Ctrl Pts',(7.09978773046573,1.58921963114407,0.205603291426271));
#16403=CARTESIAN_POINT('Ctrl Pts',(7.09638917617828,1.57844441922713,0.411206582852543));
#16404=CARTESIAN_POINT('Ctrl Pts',(7.09299062189083,1.5676692073102,0.616809874278814));
#16405=CARTESIAN_POINT('Ctrl Pts',(10.5166159648474,1.4155315881283,0.));
#16406=CARTESIAN_POINT('Ctrl Pts',(10.5064062201588,1.40475637621136,0.205603291426271));
#16407=CARTESIAN_POINT('Ctrl Pts',(10.4961964754701,1.39398116429443,0.411206582852543));
#16408=CARTESIAN_POINT('Ctrl Pts',(10.4859867307814,1.38320595237749,0.616809874278814));
#16409=CARTESIAN_POINT('Origin',(10.8,1.4,0.));
#16410=CARTESIAN_POINT('',(0.,0.,0.));
#16411=CARTESIAN_POINT('Origin',(0.,0.,0.));
#16412=CARTESIAN_POINT('',(-0.14652705620645,9.44412402177196E-5,0.0160655045842905));
#16413=CARTESIAN_POINT('',(-0.146479946776166,0.000162062070299865,0.00893449541571059));
#16414=CARTESIAN_POINT('',(-0.14635,-1.79227059055215E-17,0.));
#16415=CARTESIAN_POINT('',(0.0634007094575209,0.131904027763685,0.));
#16416=CARTESIAN_POINT('Ctrl Pts',(-0.14652705620645,9.44412402177196E-5,
0.0160655045842905));
#16417=CARTESIAN_POINT('Ctrl Pts',(-0.146560923555419,0.00502618404349199,
0.0157963945919035));
#16418=CARTESIAN_POINT('Ctrl Pts',(-0.146333578783787,0.00995455679532004,
0.0155272845995164));
#16419=CARTESIAN_POINT('Ctrl Pts',(-0.14583475180505,0.0148550342388422,
0.0152581746071293));
#16420=CARTESIAN_POINT('Ctrl Pts',(-0.140929468554047,0.0630445487404258,
0.0126118447280274));
#16421=CARTESIAN_POINT('Ctrl Pts',(-0.10977174472993,0.108536575508351,
0.0099655148489255));
#16422=CARTESIAN_POINT('Ctrl Pts',(-0.0666135938566871,0.13056551637767,
0.00731918496982359));
#16423=CARTESIAN_POINT('Ctrl Pts',(-0.0268248419338395,0.150874636338504,
0.00487945664654906));
#16424=CARTESIAN_POINT('Ctrl Pts',(0.0231637104697219,0.151241233100125,
0.00243972832327453));
#16425=CARTESIAN_POINT('Ctrl Pts',(0.0635546915223951,0.132092229195826,
-2.16840434497101E-19));
#16426=CARTESIAN_POINT('',(-0.0634007094575146,0.131904027763688,0.));
#16427=CARTESIAN_POINT('Origin',(0.,0.,0.));
#16428=CARTESIAN_POINT('Ctrl Pts',(-0.0634007094575145,0.131904027763688,
-3.88578058618805E-16));
#16429=CARTESIAN_POINT('Ctrl Pts',(-0.107282641710421,0.110811831533068,
0.00264738937425961));
#16430=CARTESIAN_POINT('Ctrl Pts',(-0.139432201149969,0.0662847592091173,
0.00529477874851962));
#16431=CARTESIAN_POINT('Ctrl Pts',(-0.145436119191498,0.0182745223106641,
0.00794216812277962));
#16432=CARTESIAN_POINT('Ctrl Pts',(-0.146186273512714,0.0122759249909008,
0.00827294388708994));
#16433=CARTESIAN_POINT('Ctrl Pts',(-0.146528267289359,0.00622295186417552,
0.00860371965140026));
#16434=CARTESIAN_POINT('Ctrl Pts',(-0.146479946776166,0.000162062070299865,
0.00893449541571059));
#16435=CARTESIAN_POINT('Origin',(0.,0.,0.));
#16436=CARTESIAN_POINT('',(-0.146148830924315,7.59978318484386E-5,0.0660655045842905));
#16437=CARTESIAN_POINT('',(-0.146133770585873,6.2751561688711E-5,0.0589344954157103));
#16438=CARTESIAN_POINT('',(-0.14635,-1.79227059055215E-17,0.));
#16439=CARTESIAN_POINT('Ctrl Pts',(-0.146148830924315,7.59978318484386E-5,
0.0660655045842905));
#16440=CARTESIAN_POINT('Ctrl Pts',(-0.146240443598182,0.0195917497831913,
0.0650077071998482));
#16441=CARTESIAN_POINT('Ctrl Pts',(-0.142607114239671,0.0390747476468127,
0.0639499098154059));
#16442=CARTESIAN_POINT('Ctrl Pts',(-0.135087779856993,0.056920264102034,
0.0628921124309636));
#16443=CARTESIAN_POINT('Ctrl Pts',(-0.116276389754784,0.10156503643559,
0.0602457825518617));
#16444=CARTESIAN_POINT('Ctrl Pts',(-0.073143724514267,0.135961331060063,
0.0575994526727599));
#16445=CARTESIAN_POINT('Ctrl Pts',(-0.025432083612881,0.144366623974243,
0.054953122793658));
#16446=CARTESIAN_POINT('Ctrl Pts',(0.0222795572885053,0.152771916888423,
0.0523067929145561));
#16447=CARTESIAN_POINT('Ctrl Pts',(0.0745701738507606,0.135186208092309,
0.0496604630354541));
#16448=CARTESIAN_POINT('Ctrl Pts',(0.107505148494886,0.0996564726649905,
0.0470141331563522));
#16449=CARTESIAN_POINT('Ctrl Pts',(0.140440123139012,0.0641267372376721,
0.0443678032772503));
#16450=CARTESIAN_POINT('Ctrl Pts',(0.154019455865009,0.010652975179149,
0.0417214733981484));
#16451=CARTESIAN_POINT('Ctrl Pts',(0.14202839331759,-0.0362847016460775,
0.0390751435190465));
#16452=CARTESIAN_POINT('Ctrl Pts',(0.130037330770172,-0.0832223784713041,
0.0364288136399446));
#16453=CARTESIAN_POINT('Ctrl Pts',(0.0924758729493388,-0.123623970063234,
0.0337824837608427));
#16454=CARTESIAN_POINT('Ctrl Pts',(0.0465351214488668,-0.139005253038876,
0.0311361538817407));
#16455=CARTESIAN_POINT('Ctrl Pts',(0.000594369948394902,-0.154386536014517,
0.0284898240026388));
#16456=CARTESIAN_POINT('Ctrl Pts',(-0.0537256752317158,-0.144747510373871,
0.025843494123537));
#16457=CARTESIAN_POINT('Ctrl Pts',(-0.0915592764828275,-0.114484496435928,
0.0231971642444351));
#16458=CARTESIAN_POINT('Ctrl Pts',(-0.125545511528741,-0.0872989822136326,
0.0208199443577202));
#16459=CARTESIAN_POINT('Ctrl Pts',(-0.146227884351973,-0.0434707826450544,
0.0184427244710054));
#16460=CARTESIAN_POINT('Ctrl Pts',(-0.14652705620645,9.44412402177196E-5,
0.0160655045842905));
#16461=CARTESIAN_POINT('Ctrl Pts',(-0.146479946776166,0.000162062070299865,
0.00893449541571059));
#16462=CARTESIAN_POINT('Ctrl Pts',(-0.146141530330399,-0.0422858476614564,
0.0112511090256603));
#16463=CARTESIAN_POINT('Ctrl Pts',(-0.126658161292025,-0.0851220706608281,
0.0135677226356099));
#16464=CARTESIAN_POINT('Ctrl Pts',(-0.0941604943243988,-0.112386678841155,
0.0158843362455596));
#16465=CARTESIAN_POINT('Ctrl Pts',(-0.0570226747722624,-0.143544241621566,
0.0185317256198196));
#16466=CARTESIAN_POINT('Ctrl Pts',(-0.00288875902448078,-0.154365965709432,
0.0211791149940796));
#16467=CARTESIAN_POINT('Ctrl Pts',(0.0434083729543798,-0.140002007265973,
0.0238265043683396));
#16468=CARTESIAN_POINT('Ctrl Pts',(0.0897055049332404,-0.125638048822514,
0.0264738937425996));
#16469=CARTESIAN_POINT('Ctrl Pts',(0.12816585314318,-0.0860884078477292,
0.0291212831168596));
#16470=CARTESIAN_POINT('Ctrl Pts',(0.141191617966992,-0.0394144013492358,
0.0317686724911196));
#16471=CARTESIAN_POINT('Ctrl Pts',(0.154217382790803,0.00725960514925768,
0.0344160618653796));
#16472=CARTESIAN_POINT('Ctrl Pts',(0.141808564228487,0.0610579771714599,
0.0370634512396396));
#16473=CARTESIAN_POINT('Ctrl Pts',(0.109639063769471,0.0973098477439542,
0.0397108406138996));
#16474=CARTESIAN_POINT('Ctrl Pts',(0.0774695633104545,0.133561718316448,
0.0423582299881596));
#16475=CARTESIAN_POINT('Ctrl Pts',(0.0255393809547383,0.152267087439235,
0.0450056193624196));
#16476=CARTESIAN_POINT('Ctrl Pts',(-0.0223595433272462,0.144872892294413,
0.0476530087366796));
#16477=CARTESIAN_POINT('Ctrl Pts',(-0.070258467609231,0.137478697149591,
0.0503003981109396));
#16478=CARTESIAN_POINT('Ctrl Pts',(-0.114126133817484,0.10398493773716,
0.0529477874851996));
#16479=CARTESIAN_POINT('Ctrl Pts',(-0.133871661545403,0.059725601630819,
0.0555951768594596));
#16480=CARTESIAN_POINT('Ctrl Pts',(-0.142173753131161,0.0411165744656389,
0.0567082830448765));
#16481=CARTESIAN_POINT('Ctrl Pts',(-0.146211489678532,0.0206043892842972,
0.0578213892302934));
#16482=CARTESIAN_POINT('Ctrl Pts',(-0.146133770585873,6.2751561688711E-5,
0.0589344954157103));
#16483=CARTESIAN_POINT('Origin',(0.,0.,0.));
#16484=CARTESIAN_POINT('',(-0.146252097264499,-0.000124487410312429,0.116065504584291));
#16485=CARTESIAN_POINT('',(-0.146276374479508,-0.000129480650117819,0.10893449541571));
#16486=CARTESIAN_POINT('',(-0.14635,-1.79227059055215E-17,0.));
#16487=CARTESIAN_POINT('Ctrl Pts',(-0.146252097264499,-0.000124487410312429,
0.116065504584291));
#16488=CARTESIAN_POINT('Ctrl Pts',(-0.145977101830714,0.0338815411246725,
0.114219019807793));
#16489=CARTESIAN_POINT('Ctrl Pts',(-0.134160879762789,0.0680598926014691,
0.112372535031295));
#16490=CARTESIAN_POINT('Ctrl Pts',(-0.112484833627769,0.0939988017516943,
0.110526050254798));
#16491=CARTESIAN_POINT('Ctrl Pts',(-0.0814193359437304,0.131173714423195,
0.107879720375696));
#16492=CARTESIAN_POINT('Ctrl Pts',(-0.0301019434218634,0.151424966146533,
0.105233390496594));
#16493=CARTESIAN_POINT('Ctrl Pts',(0.0179785702873004,0.145483266051774,
0.102587060617492));
#16494=CARTESIAN_POINT('Ctrl Pts',(0.0660590839964643,0.139541565957016,
0.0999407307383904));
#16495=CARTESIAN_POINT('Ctrl Pts',(0.110902718892925,0.107406914044162,
0.0972944008592884));
#16496=CARTESIAN_POINT('Ctrl Pts',(0.131983829661647,0.0637877973597534,
0.0946480709801865));
#16497=CARTESIAN_POINT('Ctrl Pts',(0.15306494043037,0.0201686806753445,
0.0920017411010846));
#16498=CARTESIAN_POINT('Ctrl Pts',(0.150383527071356,-0.0349349007806195,
0.0893554112219828));
#16499=CARTESIAN_POINT('Ctrl Pts',(0.125166930059577,-0.0763010783846813,
0.0867090813428809));
#16500=CARTESIAN_POINT('Ctrl Pts',(0.0999503330477985,-0.117667255988743,
0.084062751463779));
#16501=CARTESIAN_POINT('Ctrl Pts',(0.0521985523832557,-0.145296029740903,
0.081416421584677));
#16502=CARTESIAN_POINT('Ctrl Pts',(0.00376830011669856,-0.146541450754272,
0.0787700917055751));
#16503=CARTESIAN_POINT('Ctrl Pts',(-0.0446619521498586,-0.147786871767642,
0.0761237618264732));
#16504=CARTESIAN_POINT('Ctrl Pts',(-0.09377067601843,-0.122648940042221,
0.0734774319473713));
#16505=CARTESIAN_POINT('Ctrl Pts',(-0.121079980470766,-0.0826333491581908,
0.0708311020682694));
#16506=CARTESIAN_POINT('Ctrl Pts',(-0.137473143648068,-0.0586128871159229,
0.0692425695736098));
#16507=CARTESIAN_POINT('Ctrl Pts',(-0.146011252866834,-0.02923151094855,
0.0676540370789502));
#16508=CARTESIAN_POINT('Ctrl Pts',(-0.146148830924315,7.59978318484386E-5,
0.0660655045842905));
#16509=CARTESIAN_POINT('Ctrl Pts',(-0.146133770585873,6.2751561688711E-5,
0.0589344954157103));
#16510=CARTESIAN_POINT('Ctrl Pts',(-0.146026644150963,-0.0282514289199324,
0.0604687786045534));
#16511=CARTESIAN_POINT('Ctrl Pts',(-0.138100435392092,-0.0566215672018456,
0.0620030617933965));
#16512=CARTESIAN_POINT('Ctrl Pts',(-0.122745086057252,-0.0801407530065182,
0.0635373449822396));
#16513=CARTESIAN_POINT('Ctrl Pts',(-0.0962495935935968,-0.120722858737265,
0.0661847343564996));
#16514=CARTESIAN_POINT('Ctrl Pts',(-0.0476352194187008,-0.146862157398507,
0.0688321237307596));
#16515=CARTESIAN_POINT('Ctrl Pts',(0.00082938917649622,-0.146587691816784,
0.0714795131050196));
#16516=CARTESIAN_POINT('Ctrl Pts',(0.0492939977716932,-0.146313226235061,
0.0741269024792796));
#16517=CARTESIAN_POINT('Ctrl Pts',(0.0976088407871913,-0.119624996410372,
0.0767742918535397));
#16518=CARTESIAN_POINT('Ctrl Pts',(0.123643642180798,-0.0787464320231966,
0.0794216812277997));
#16519=CARTESIAN_POINT('Ctrl Pts',(0.149678443574405,-0.0378678676360213,
0.0820690706020596));
#16520=CARTESIAN_POINT('Ctrl Pts',(0.153433203346121,0.0172010313136401,
0.0847164599763195));
#16521=CARTESIAN_POINT('Ctrl Pts',(0.133187835944515,0.06123527443138,0.0873638493505795));
#16522=CARTESIAN_POINT('Ctrl Pts',(0.11294246854291,0.10526951754912,0.0900112387248395));
#16523=CARTESIAN_POINT('Ctrl Pts',(0.0686969739679828,0.138269104834938,
0.0926586280990997));
#16524=CARTESIAN_POINT('Ctrl Pts',(0.0207181735233275,0.145118849380084,
0.0953060174733597));
#16525=CARTESIAN_POINT('Ctrl Pts',(-0.027260626921328,0.151968593925229,
0.0979534068476197));
#16526=CARTESIAN_POINT('Ctrl Pts',(-0.0789727332357116,0.132668495729702,
0.10060079622188));
#16527=CARTESIAN_POINT('Ctrl Pts',(-0.110731403441959,0.0960588230543748,
0.10324818559614));
#16528=CARTESIAN_POINT('Ctrl Pts',(-0.133469481440122,0.0698475998711364,
0.105143622202663));
#16529=CARTESIAN_POINT('Ctrl Pts',(-0.145979327216774,0.0347634013028336,
0.107039058809187));
#16530=CARTESIAN_POINT('Ctrl Pts',(-0.146276374479508,-0.000129480650117819,
0.10893449541571));
#16531=CARTESIAN_POINT('Origin',(0.,0.,0.));
#16532=CARTESIAN_POINT('',(-0.146589818999335,-3.81787486967988E-6,0.166065504584291));
#16533=CARTESIAN_POINT('',(-0.146589453522336,1.04004190909306E-5,0.15893449541571));
#16534=CARTESIAN_POINT('',(-0.14635,-1.79227059055215E-17,0.));
#16535=CARTESIAN_POINT('Ctrl Pts',(-0.146589818999335,-3.81787486967988E-6,
0.166065504584291));
#16536=CARTESIAN_POINT('Ctrl Pts',(-0.146571339149733,0.0482382848470949,
0.163430332415738));
#16537=CARTESIAN_POINT('Ctrl Pts',(-0.120433071521034,0.0964975486977609,
0.160795160247185));
#16538=CARTESIAN_POINT('Ctrl Pts',(-0.0800107885095625,0.122828684230981,
0.158159988078632));
#16539=CARTESIAN_POINT('Ctrl Pts',(-0.0394173515450545,0.149271309704865,
0.15551365819953));
#16540=CARTESIAN_POINT('Ctrl Pts',(0.0155813181737399,0.153599719825856,
0.152867328320428));
#16541=CARTESIAN_POINT('Ctrl Pts',(0.0598114643267532,0.133832733731537,
0.150220998441327));
#16542=CARTESIAN_POINT('Ctrl Pts',(0.104041610479766,0.114065747637217,
0.147574668562225));
#16543=CARTESIAN_POINT('Ctrl Pts',(0.137503233066998,0.0702033653275883,
0.144928338683123));
#16544=CARTESIAN_POINT('Ctrl Pts',(0.144880420813362,0.0223220882221681,
0.142282008804021));
#16545=CARTESIAN_POINT('Ctrl Pts',(0.152257608559726,-0.0255591888832524,
0.139635678924919));
#16546=CARTESIAN_POINT('Ctrl Pts',(0.133550361465222,-0.077459360784464,
0.136989349045817));
#16547=CARTESIAN_POINT('Ctrl Pts',(0.0973212811704284,-0.109622900294719,
0.134343019166715));
#16548=CARTESIAN_POINT('Ctrl Pts',(0.0610922008756344,-0.141786439804975,
0.131696689287613));
#16549=CARTESIAN_POINT('Ctrl Pts',(0.00734128738055008,-0.154213346924274,
0.129050359408511));
#16550=CARTESIAN_POINT('Ctrl Pts',(-0.0393288211819405,-0.141215634503184,
0.126404029529409));
#16551=CARTESIAN_POINT('Ctrl Pts',(-0.0859989297444312,-0.128217922082094,
0.123757699650308));
#16552=CARTESIAN_POINT('Ctrl Pts',(-0.125588233374328,-0.0897955901206149,
0.121111369771206));
#16553=CARTESIAN_POINT('Ctrl Pts',(-0.139976083766172,-0.043535137330043,
0.118465039892104));
#16554=CARTESIAN_POINT('Ctrl Pts',(-0.144324767489921,-0.0295530571287048,
0.117665194789499));
#16555=CARTESIAN_POINT('Ctrl Pts',(-0.146371217526823,-0.0148549394177889,
0.116865349686895));
#16556=CARTESIAN_POINT('Ctrl Pts',(-0.146252097264499,-0.000124487410312429,
0.116065504584291));
#16557=CARTESIAN_POINT('Ctrl Pts',(-0.146276374479508,-0.000129480650117819,
0.10893449541571));
#16558=CARTESIAN_POINT('Ctrl Pts',(-0.14639421831063,-0.0139720956278579,
0.109686448183447));
#16559=CARTESIAN_POINT('Ctrl Pts',(-0.14458995413065,-0.0277846002915201,
0.110438400951183));
#16560=CARTESIAN_POINT('Ctrl Pts',(-0.140739671041232,-0.041001045008257,
0.11119035371892));
#16561=CARTESIAN_POINT('Ctrl Pts',(-0.127184034336146,-0.0875319932404337,
0.11383774309318));
#16562=CARTESIAN_POINT('Ctrl Pts',(-0.0882675268278623,-0.12667464254966,
0.11648513246744));
#16563=CARTESIAN_POINT('Ctrl Pts',(-0.0418159243469935,-0.140499695546946,
0.1191325218417));
#16564=CARTESIAN_POINT('Ctrl Pts',(0.00463567813387508,-0.154324748544231,
0.12177991121596));
#16565=CARTESIAN_POINT('Ctrl Pts',(0.0586223755873289,-0.142832205229577,
0.12442730059022));
#16566=CARTESIAN_POINT('Ctrl Pts',(0.0954154960694136,-0.111286216216264,
0.12707468996448));
#16567=CARTESIAN_POINT('Ctrl Pts',(0.132208616551499,-0.0797402272029501,
0.12972207933874));
#16568=CARTESIAN_POINT('Ctrl Pts',(0.151808160062214,-0.0281407924909768,
0.132369468712999));
#16569=CARTESIAN_POINT('Ctrl Pts',(0.145236524363737,0.0198768833792122,
0.135016858087259));
#16570=CARTESIAN_POINT('Ctrl Pts',(0.138664888665259,0.0678945592494009,
0.13766424746152));
#16571=CARTESIAN_POINT('Ctrl Pts',(0.105922073757589,0.112330476277805,
0.14031163683578));
#16572=CARTESIAN_POINT('Ctrl Pts',(0.062005973158836,0.132830708741579,
0.14295902621004));
#16573=CARTESIAN_POINT('Ctrl Pts',(0.0180898725600832,0.153330941205352,
0.1456064155843));
#16574=CARTESIAN_POINT('Ctrl Pts',(-0.0369995137297515,0.149895489104495,
0.14825380495856));
#16575=CARTESIAN_POINT('Ctrl Pts',(-0.0780284182758478,0.124097962381086,
0.15090119433282));
#16576=CARTESIAN_POINT('Ctrl Pts',(-0.119057322821944,0.0983004356576776,
0.153548583707079));
#16577=CARTESIAN_POINT('Ctrl Pts',(-0.146025745624302,0.0501408343117172,
0.15619597308134));
#16578=CARTESIAN_POINT('Ctrl Pts',(-0.14658076309025,0.00167873146180186,
0.1588433624556));
#16579=CARTESIAN_POINT('Ctrl Pts',(-0.146587131676737,0.00112264969450139,
0.15887374010897));
#16580=CARTESIAN_POINT('Ctrl Pts',(-0.146590022522527,0.000566528098114988,
0.15890411776234));
#16581=CARTESIAN_POINT('Ctrl Pts',(-0.146589453522336,1.04004190909306E-5,
0.15893449541571));
#16582=CARTESIAN_POINT('Origin',(0.,0.,0.));
#16583=CARTESIAN_POINT('',(-0.146263250741535,0.000126870157254357,0.21606550458429));
#16584=CARTESIAN_POINT('',(-0.146245769975643,0.000123264779366826,0.20893449541571));
#16585=CARTESIAN_POINT('',(-0.14635,-1.79227059055215E-17,0.));
#16586=CARTESIAN_POINT('Ctrl Pts',(-0.146263250741535,0.000126870157254357,
0.21606550458429));
#16587=CARTESIAN_POINT('Ctrl Pts',(-0.146381923100139,0.0144435832128767,
0.215287974902784));
#16588=CARTESIAN_POINT('Ctrl Pts',(-0.144450237714319,0.0287289633064517,
0.214510445221278));
#16589=CARTESIAN_POINT('Ctrl Pts',(-0.140337374518256,0.0423560295890773,
0.213732915539772));
#16590=CARTESIAN_POINT('Ctrl Pts',(-0.126339204386259,0.0887358830222778,
0.21108658566067));
#16591=CARTESIAN_POINT('Ctrl Pts',(-0.0870745347363382,0.127489909020004,
0.208440255781569));
#16592=CARTESIAN_POINT('Ctrl Pts',(-0.0405154226099946,0.140879780169064,
0.205793925902467));
#16593=CARTESIAN_POINT('Ctrl Pts',(0.00604368951634975,0.154269651318124,
0.203147596023365));
#16594=CARTESIAN_POINT('Ctrl Pts',(0.0598972441191175,0.142295367618517,
0.200501266144263));
#16595=CARTESIAN_POINT('Ctrl Pts',(0.0963956219934077,0.110437747119808,
0.197854936265161));
#16596=CARTESIAN_POINT('Ctrl Pts',(0.132893999867697,0.0785801266211,0.195208606386059));
#16597=CARTESIAN_POINT('Ctrl Pts',(0.15203720101351,0.0268391693232909,
0.192562276506957));
#16598=CARTESIAN_POINT('Ctrl Pts',(0.145063081087281,-0.0211024746124516,
0.189915946627855));
#16599=CARTESIAN_POINT('Ctrl Pts',(0.138088961161051,-0.0690441185481943,
0.187269616748753));
#16600=CARTESIAN_POINT('Ctrl Pts',(0.10499752016278,-0.11318644912187,0.184623286869651));
#16601=CARTESIAN_POINT('Ctrl Pts',(0.060935231264163,-0.133324827106958,
0.181976956990549));
#16602=CARTESIAN_POINT('Ctrl Pts',(0.0168729423655461,-0.153463205092045,
0.179330627111448));
#16603=CARTESIAN_POINT('Ctrl Pts',(-0.0381601944334158,-0.149597630488544,
0.176684297232346));
#16604=CARTESIAN_POINT('Ctrl Pts',(-0.0789746466099193,-0.123497437688695,
0.174037967353244));
#16605=CARTESIAN_POINT('Ctrl Pts',(-0.119961184605052,-0.0972871987457574,
0.171380479763593));
#16606=CARTESIAN_POINT('Ctrl Pts',(-0.146608455341797,-0.0486544490602708,
0.168722992173942));
#16607=CARTESIAN_POINT('Ctrl Pts',(-0.146589818999335,-3.81787486967988E-6,
0.166065504584291));
#16608=CARTESIAN_POINT('Ctrl Pts',(-0.146589453522336,1.04004190909306E-5,
0.15893449541571));
#16609=CARTESIAN_POINT('Ctrl Pts',(-0.146540434588914,-0.0478995759235739,
0.1615515071366));
#16610=CARTESIAN_POINT('Ctrl Pts',(-0.120813506558866,-0.0958546957256878,
0.16416851885749));
#16611=CARTESIAN_POINT('Ctrl Pts',(-0.0808500697395765,-0.122278388912248,
0.16678553057838));
#16612=CARTESIAN_POINT('Ctrl Pts',(-0.0404227467934142,-0.149008802082514,
0.16943291995264));
#16613=CARTESIAN_POINT('Ctrl Pts',(0.0145735112284506,-0.153705024069172,
0.1720803093269));
#16614=CARTESIAN_POINT('Ctrl Pts',(0.0589475933459444,-0.134215943447351,
0.17472769870116));
#16615=CARTESIAN_POINT('Ctrl Pts',(0.103321675463438,-0.11472686282553,
0.17737508807542));
#16616=CARTESIAN_POINT('Ctrl Pts',(0.137073581676561,-0.0710524795952304,
0.18002247744968));
#16617=CARTESIAN_POINT('Ctrl Pts',(0.144743205110219,-0.0231979049720499,
0.18266986682394));
#16618=CARTESIAN_POINT('Ctrl Pts',(0.152412828543877,0.024656669651131,
0.1853172561982));
#16619=CARTESIAN_POINT('Ctrl Pts',(0.13400016919807,0.0766914356671922,
0.18796464557246));
#16620=CARTESIAN_POINT('Ctrl Pts',(0.0979391709064228,0.109071797518936,
0.19061203494672));
#16621=CARTESIAN_POINT('Ctrl Pts',(0.0618781726147763,0.141452159370678,
0.19325942432098));
#16622=CARTESIAN_POINT('Ctrl Pts',(0.00816883537729064,0.154178117058104,
0.195906813695239));
#16623=CARTESIAN_POINT('Ctrl Pts',(-0.0385872054932313,0.1414205281901,
0.198554203069499));
#16624=CARTESIAN_POINT('Ctrl Pts',(-0.0853432463637543,0.128662939322095,
0.201201592443759));
#16625=CARTESIAN_POINT('Ctrl Pts',(-0.125145990867313,0.0904218038986596,
0.20384898181802));
#16626=CARTESIAN_POINT('Ctrl Pts',(-0.139763737461459,0.0442135263146365,
0.20649637119228));
#16627=CARTESIAN_POINT('Ctrl Pts',(-0.144251162244238,0.030028291356252,
0.207309079266757));
#16628=CARTESIAN_POINT('Ctrl Pts',(-0.146365162502875,0.0150922359825044,
0.208121787341234));
#16629=CARTESIAN_POINT('Ctrl Pts',(-0.146245769975643,0.000123264779366826,
0.20893449541571));
#16630=CARTESIAN_POINT('Origin',(0.,0.,0.));
#16631=CARTESIAN_POINT('',(-0.146142672279203,-7.01165389862951E-5,0.266065504584291));
#16632=CARTESIAN_POINT('',(-0.146150215784492,-7.74481165901552E-5,0.258934495415711));
#16633=CARTESIAN_POINT('',(-0.14635,-1.79227059055215E-17,0.));
#16634=CARTESIAN_POINT('Ctrl Pts',(-0.146142672279203,-7.01165389862951E-5,
0.266065504584291));
#16635=CARTESIAN_POINT('Ctrl Pts',(-0.146017527260215,0.028828671850369,
0.264499287510729));
#16636=CARTESIAN_POINT('Ctrl Pts',(-0.137733916992107,0.0577936173630845,
0.262933070437168));
#16637=CARTESIAN_POINT('Ctrl Pts',(-0.121770841384076,0.0816117278206753,
0.261366853363607));
#16638=CARTESIAN_POINT('Ctrl Pts',(-0.0947991242083451,0.121855560193383,
0.258720523484505));
#16639=CARTESIAN_POINT('Ctrl Pts',(-0.0459036471244643,0.147405924851771,
0.256074193605403));
#16640=CARTESIAN_POINT('Ctrl Pts',(0.0025353607453442,0.146568017913755,
0.253427863726301));
#16641=CARTESIAN_POINT('Ctrl Pts',(0.050974368615152,0.145730110975738,
0.250781533847199));
#16642=CARTESIAN_POINT('Ctrl Pts',(0.0989569072708876,0.118503932441319,
0.248135203968097));
#16643=CARTESIAN_POINT('Ctrl Pts',(0.124520613871998,0.0773513325689396,
0.245488874088995));
#16644=CARTESIAN_POINT('Ctrl Pts',(0.150084320473109,0.0361987326965595,
0.242842544209893));
#16645=CARTESIAN_POINT('Ctrl Pts',(0.153229195019594,-0.0188802885137813,
0.240196214330791));
#16646=CARTESIAN_POINT('Ctrl Pts',(0.132515778953886,-0.0626751965094481,
0.237549884451689));
#16647=CARTESIAN_POINT('Ctrl Pts',(0.111802362888177,-0.106470104505115,
0.234903554572587));
#16648=CARTESIAN_POINT('Ctrl Pts',(0.0672306562102751,-0.138980899286108,
0.232257224693486));
#16649=CARTESIAN_POINT('Ctrl Pts',(0.0192018303028616,-0.145326878595667,
0.229610894814384));
#16650=CARTESIAN_POINT('Ctrl Pts',(-0.0288269956045516,-0.151672857905225,
0.226964564935282));
#16651=CARTESIAN_POINT('Ctrl Pts',(-0.0803129407414762,-0.131854021743351,
0.22431823505618));
#16652=CARTESIAN_POINT('Ctrl Pts',(-0.111690078002902,-0.0949417632280756,
0.221671905177078));
#16653=CARTESIAN_POINT('Ctrl Pts',(-0.133848162215005,-0.0688748557907962,
0.219803104979482));
#16654=CARTESIAN_POINT('Ctrl Pts',(-0.145978020566425,-0.0342834897603843,
0.217934304781886));
#16655=CARTESIAN_POINT('Ctrl Pts',(-0.146263250741535,0.000126870157254357,
0.21606550458429));
#16656=CARTESIAN_POINT('Ctrl Pts',(-0.146245769975643,0.000123264779366826,
0.20893449541571));
#16657=CARTESIAN_POINT('Ctrl Pts',(-0.145976242399967,-0.03366905549635,
0.210769176715493));
#16658=CARTESIAN_POINT('Ctrl Pts',(-0.134324750276972,-0.067629123606452,
0.212603858015276));
#16659=CARTESIAN_POINT('Ctrl Pts',(-0.112902327433,-0.0934976078712483,
0.214438539315059));
#16660=CARTESIAN_POINT('Ctrl Pts',(-0.0819904221256615,-0.130825044728502,
0.217085928689319));
#16661=CARTESIAN_POINT('Ctrl Pts',(-0.0307338628262512,-0.151304498698398,
0.21973331806358));
#16662=CARTESIAN_POINT('Ctrl Pts',(0.0173892134168267,-0.145555327884408,
0.22238070743784));
#16663=CARTESIAN_POINT('Ctrl Pts',(0.0655122896599044,-0.139806157070418,
0.2250280968121));
#16664=CARTESIAN_POINT('Ctrl Pts',(0.11050188284665,-0.107828361472542,
0.22767548618636));
#16665=CARTESIAN_POINT('Ctrl Pts',(0.131750448317205,-0.0642694140823833,
0.23032287556062));
#16666=CARTESIAN_POINT('Ctrl Pts',(0.15299901378776,-0.020710466692225,
0.232970264934879));
#16667=CARTESIAN_POINT('Ctrl Pts',(0.150506551542124,0.0344296324902152,
0.23561765430914));
#16668=CARTESIAN_POINT('Ctrl Pts',(0.125414737320077,0.0758938856636754,
0.2382650436834));
#16669=CARTESIAN_POINT('Ctrl Pts',(0.10032292309803,0.117358138837136,0.24091243305766));
#16670=CARTESIAN_POINT('Ctrl Pts',(0.0526317568995709,0.145146546001616,
0.24355982243192));
#16671=CARTESIAN_POINT('Ctrl Pts',(0.00418624259284972,0.146530589268381,
0.24620721180618));
#16672=CARTESIAN_POINT('Ctrl Pts',(-0.0442592717138715,0.147914632535146,
0.24885460118044));
#16673=CARTESIAN_POINT('Ctrl Pts',(-0.0934591341288551,0.122894311904195,
0.2515019905547));
#16674=CARTESIAN_POINT('Ctrl Pts',(-0.120877280418781,0.082930219442967,
0.25414937992896));
#16675=CARTESIAN_POINT('Ctrl Pts',(-0.137396572682769,0.0588520590724165,
0.255744418424543));
#16676=CARTESIAN_POINT('Ctrl Pts',(-0.146009100715185,0.0293493086505574,
0.257339456920127));
#16677=CARTESIAN_POINT('Ctrl Pts',(-0.146150215784492,-7.74481165901552E-5,
0.258934495415711));
#16678=CARTESIAN_POINT('Origin',(0.,0.,0.));
#16679=CARTESIAN_POINT('',(-0.146519404976022,-8.97763884284003E-5,0.316065504584291));
#16680=CARTESIAN_POINT('',(-0.146528765763263,-8.45393868379275E-5,0.30893449541571));
#16681=CARTESIAN_POINT('',(-0.14635,-1.79227059055215E-17,0.));
#16682=CARTESIAN_POINT('Ctrl Pts',(-0.146519404976022,-8.97763884284003E-5,
0.316065504584291));
#16683=CARTESIAN_POINT('Ctrl Pts',(-0.146208092107557,0.043076445171776,
0.313710600118674));
#16684=CARTESIAN_POINT('Ctrl Pts',(-0.125958424314353,0.0864965766126209,
0.311355695653057));
#16685=CARTESIAN_POINT('Ctrl Pts',(-0.0925183485457987,0.1137056160074,
0.309000791187441));
#16686=CARTESIAN_POINT('Ctrl Pts',(-0.0549399784004991,0.144281843189175,
0.306354461308339));
#16687=CARTESIAN_POINT('Ctrl Pts',(-0.00070450021881692,0.154386382754941,
0.303708131429237));
#16688=CARTESIAN_POINT('Ctrl Pts',(0.0453636543616171,0.139394227973128,
0.301061801550135));
#16689=CARTESIAN_POINT('Ctrl Pts',(0.0914318089420511,0.124402073191315,
0.298415471671033));
#16690=CARTESIAN_POINT('Ctrl Pts',(0.129332639921237,0.0843132240619223,
0.295769141791931));
#16691=CARTESIAN_POINT('Ctrl Pts',(0.141718340675246,0.0374769775398043,
0.293122811912829));
#16692=CARTESIAN_POINT('Ctrl Pts',(0.154104041429255,-0.00935926898231351,
0.290476482033727));
#16693=CARTESIAN_POINT('Ctrl Pts',(0.140974611958088,-0.0629429128971569,
0.287830152154626));
#16694=CARTESIAN_POINT('Ctrl Pts',(0.108339598692885,-0.0987478773661917,
0.285183822275524));
#16695=CARTESIAN_POINT('Ctrl Pts',(0.0757045854276824,-0.134552841835227,
0.282537492396422));
#16696=CARTESIAN_POINT('Ctrl Pts',(0.0235639883684441,-0.152579126858453,
0.27989116251732));
#16697=CARTESIAN_POINT('Ctrl Pts',(-0.0242166208952047,-0.144575818177467,
0.277244832638218));
#16698=CARTESIAN_POINT('Ctrl Pts',(-0.0719972301588528,-0.136572509496481,
0.274598502759116));
#16699=CARTESIAN_POINT('Ctrl Pts',(-0.115417851626912,-0.102539607111283,
0.271952172880014));
#16700=CARTESIAN_POINT('Ctrl Pts',(-0.13460418372715,-0.0580545058751705,
0.269305843000912));
#16701=CARTESIAN_POINT('Ctrl Pts',(-0.142435181350113,-0.0398976888130428,
0.268225730195372));
#16702=CARTESIAN_POINT('Ctrl Pts',(-0.146228976240411,-0.0199996345674016,
0.267145617389831));
#16703=CARTESIAN_POINT('Ctrl Pts',(-0.146142672279203,-7.01165389862951E-5,
0.266065504584291));
#16704=CARTESIAN_POINT('Ctrl Pts',(-0.146150215784492,-7.74481165901552E-5,
0.258934495415711));
#16705=CARTESIAN_POINT('Ctrl Pts',(-0.146243318595233,-0.0194921979337541,
0.259986846294387));
#16706=CARTESIAN_POINT('Ctrl Pts',(-0.142648899141753,-0.0388738684647463,
0.261039197173063));
#16707=CARTESIAN_POINT('Ctrl Pts',(-0.135204796371803,-0.0566427511368837,
0.26209154805174));
#16708=CARTESIAN_POINT('Ctrl Pts',(-0.116477735870028,-0.101343764964001,
0.264738937426));
#16709=CARTESIAN_POINT('Ctrl Pts',(-0.0733871847016099,-0.135837928326728,
0.26738632680026));
#16710=CARTESIAN_POINT('Ctrl Pts',(-0.0256708287318585,-0.144325142544676,
0.27003371617452));
#16711=CARTESIAN_POINT('Ctrl Pts',(0.0220455272378925,-0.152812356762624,
0.27268110554878));
#16712=CARTESIAN_POINT('Ctrl Pts',(0.0743876880089763,-0.135292621835792,
0.27532849492304));
#16713=CARTESIAN_POINT('Ctrl Pts',(0.10738025529095,-0.0997908762961729,
0.2779758842973));
#16714=CARTESIAN_POINT('Ctrl Pts',(0.140372822572925,-0.0642891307565533,
0.280623273671559));
#16715=CARTESIAN_POINT('Ctrl Pts',(0.154015796365789,-0.010805374604146,
0.283270663045819));
#16716=CARTESIAN_POINT('Ctrl Pts',(0.142059993874458,0.0361620845457957,
0.285918052420079));
#16717=CARTESIAN_POINT('Ctrl Pts',(0.130104191383128,0.0831295436957373,
0.288565441794339));
#16718=CARTESIAN_POINT('Ctrl Pts',(0.0925496126076039,0.123580705843213,
0.291212831168599));
#16719=CARTESIAN_POINT('Ctrl Pts',(0.0465981836912963,0.138986860871753,
0.29386022054286));
#16720=CARTESIAN_POINT('Ctrl Pts',(0.000646754774988913,0.154393015900293,
0.296507609917119));
#16721=CARTESIAN_POINT('Ctrl Pts',(-0.0537015242821025,0.144754163809898,
0.29915499929138));
#16722=CARTESIAN_POINT('Ctrl Pts',(-0.0915523499663989,0.114485393976436,
0.30180238866564));
#16723=CARTESIAN_POINT('Ctrl Pts',(-0.125542580994678,0.0873038870745135,
0.30417975758233));
#16724=CARTESIAN_POINT('Ctrl Pts',(-0.146229051243382,0.0434861464246214,
0.30655712649902));
#16725=CARTESIAN_POINT('Ctrl Pts',(-0.146528765763263,-8.45393868379275E-5,
0.30893449541571));
#16726=CARTESIAN_POINT('Origin',(0.,0.,0.));
#16727=CARTESIAN_POINT('',(-0.146416087288192,0.000126442170093593,0.366065504584291));
#16728=CARTESIAN_POINT('',(-0.146408012399712,0.000128195943346294,0.358934495415711));
#16729=CARTESIAN_POINT('',(-0.14635,-1.79227059055215E-17,0.));
#16730=CARTESIAN_POINT('Ctrl Pts',(-0.146416087288192,0.000126442170093593,
0.366065504584291));
#16731=CARTESIAN_POINT('Ctrl Pts',(-0.146499294961499,0.00925816812376314,
0.365568242605721));
#16732=CARTESIAN_POINT('Ctrl Pts',(-0.145718277739785,0.0183757049974218,
0.365070980627151));
#16733=CARTESIAN_POINT('Ctrl Pts',(-0.144021710151773,0.0273195705351122,
0.364573718648581));
#16734=CARTESIAN_POINT('Ctrl Pts',(-0.134992913071845,0.0749170536065741,
0.361927388769479));
#16735=CARTESIAN_POINT('Ctrl Pts',(-0.100034284522917,0.117595890322328,
0.359281058890377));
#16736=CARTESIAN_POINT('Ctrl Pts',(-0.0551469387876206,0.135821305661589,
0.356634729011275));
#16737=CARTESIAN_POINT('Ctrl Pts',(-0.0102595930523245,0.15404672100085,
0.353988399132173));
#16738=CARTESIAN_POINT('Ctrl Pts',(0.0445564698693406,0.147818714963618,
0.351342069253072));
#16739=CARTESIAN_POINT('Ctrl Pts',(0.0842110755700531,0.119987943896873,
0.34869573937397));
#16740=CARTESIAN_POINT('Ctrl Pts',(0.123865681270766,0.0921571728301272,
0.346049409494868));
#16741=CARTESIAN_POINT('Ctrl Pts',(0.148358829750526,0.0427236367338667,
0.343403079615766));
#16742=CARTESIAN_POINT('Ctrl Pts',(0.146479621605269,-0.00568615719458776,
0.340756749736664));
#16743=CARTESIAN_POINT('Ctrl Pts',(0.144600413460012,-0.0540959511230416,
0.338110419857562));
#16744=CARTESIAN_POINT('Ctrl Pts',(0.116348848689739,-0.101482002883689,
0.33546408997846));
#16745=CARTESIAN_POINT('Ctrl Pts',(0.0746561129649502,-0.126154971072205,
0.332817760099358));
#16746=CARTESIAN_POINT('Ctrl Pts',(0.0329633772401616,-0.150827939260721,
0.330171430220256));
#16747=CARTESIAN_POINT('Ctrl Pts',(-0.0221705294391424,-0.152787823877104,
0.327525100341154));
#16748=CARTESIAN_POINT('Ctrl Pts',(-0.0655099505772086,-0.131137554898038,
0.324878770462052));
#16749=CARTESIAN_POINT('Ctrl Pts',(-0.108849371715275,-0.109487285918972,
0.322232440582951));
#16750=CARTESIAN_POINT('Ctrl Pts',(-0.140394307312104,-0.0642268633444555,
0.319586110703849));
#16751=CARTESIAN_POINT('Ctrl Pts',(-0.14570614405606,-0.0160726946583056,
0.316939780824747));
#16752=CARTESIAN_POINT('Ctrl Pts',(-0.146291106736525,-0.0107697471190636,
0.316648355411261));
#16753=CARTESIAN_POINT('Ctrl Pts',(-0.146557930734812,-0.0054317060295066,
0.316356929997776));
#16754=CARTESIAN_POINT('Ctrl Pts',(-0.146519404976022,-8.97763884284003E-5,
0.316065504584291));
#16755=CARTESIAN_POINT('Ctrl Pts',(-0.146528765763263,-8.45393868379275E-5,
0.30893449541571));
#16756=CARTESIAN_POINT('Ctrl Pts',(-0.146562807199252,-0.00503327764821679,
0.30920451587328));
#16757=CARTESIAN_POINT('Ctrl Pts',(-0.14633385314783,-0.00997882882536714,
0.30947453633085));
#16758=CARTESIAN_POINT('Ctrl Pts',(-0.145831525524598,-0.0148964553326841,
0.309744556788419));
#16759=CARTESIAN_POINT('Ctrl Pts',(-0.140906503086998,-0.0631108472318147,
0.312391946162679));
#16760=CARTESIAN_POINT('Ctrl Pts',(-0.109703085900295,-0.108640943453547,
0.31503933553694));
#16761=CARTESIAN_POINT('Ctrl Pts',(-0.0665140418604196,-0.13063162118607,
0.3176867249112));
#16762=CARTESIAN_POINT('Ctrl Pts',(-0.0233249978205455,-0.152622298918592,
0.32033411428546));
#16763=CARTESIAN_POINT('Ctrl Pts',(0.0318496730725009,-0.151073558161906,
0.322981503659719));
#16764=CARTESIAN_POINT('Ctrl Pts',(0.0737371373950496,-0.126694801736668,
0.325628893033979));
#16765=CARTESIAN_POINT('Ctrl Pts',(0.115624601717599,-0.10231604531143,
0.328276282408239));
#16766=CARTESIAN_POINT('Ctrl Pts',(0.144224859469651,-0.0551072732176397,
0.3309236717825));
#16767=CARTESIAN_POINT('Ctrl Pts',(0.146437523492708,-0.0066925280449658,
0.33357106115676));
#16768=CARTESIAN_POINT('Ctrl Pts',(0.148650187515766,0.0417222171277085,
0.33621845053102));
#16769=CARTESIAN_POINT('Ctrl Pts',(0.124475257809829,0.0913429353792657,
0.33886583990528));
#16770=CARTESIAN_POINT('Ctrl Pts',(0.0849860939726622,0.119440788885456,
0.34151322927954));
#16771=CARTESIAN_POINT('Ctrl Pts',(0.0454969301354961,0.147538642391646,
0.344160618653799));
#16772=CARTESIAN_POINT('Ctrl Pts',(-0.00930646783289898,0.154113631152469,
0.346808008028059));
#16773=CARTESIAN_POINT('Ctrl Pts',(-0.0543213285795041,0.136154072578339,
0.349455397402319));
#16774=CARTESIAN_POINT('Ctrl Pts',(-0.0993361893261098,0.11819451400421,
0.352102786776579));
#16775=CARTESIAN_POINT('Ctrl Pts',(-0.134562512850926,0.0757004080951257,
0.35475017615084));
#16776=CARTESIAN_POINT('Ctrl Pts',(-0.143864833510727,0.0281362381501331,
0.3573975655251));
#16777=CARTESIAN_POINT('Ctrl Pts',(-0.145664973529558,0.0189318504589563,
0.357909875488637));
#16778=CARTESIAN_POINT('Ctrl Pts',(-0.146494308508217,0.00953759842677947,
0.358422185452174));
#16779=CARTESIAN_POINT('Ctrl Pts',(-0.146408012399712,0.000128195943346294,
0.358934495415711));
#16780=CARTESIAN_POINT('Origin',(0.,0.,0.));
#16781=CARTESIAN_POINT('',(-0.146110491840834,1.12683595067248E-5,0.416065504584291));
#16782=CARTESIAN_POINT('',(-0.146109756335714,8.81622270207575E-6,0.40893449541571));
#16783=CARTESIAN_POINT('',(-0.14635,-1.79227059055215E-17,0.));
#16784=CARTESIAN_POINT('Ctrl Pts',(-0.146110491840834,1.12683595067248E-5,
0.416065504584291));
#16785=CARTESIAN_POINT('Ctrl Pts',(-0.146126798292857,0.0237518011834032,
0.414779555213666));
#16786=CARTESIAN_POINT('Ctrl Pts',(-0.140669750958991,0.0474852665485293,
0.413493605843041));
#16787=CARTESIAN_POINT('Ctrl Pts',(-0.129698698951591,0.0683144158983218,
0.412207656472415));
#16788=CARTESIAN_POINT('Ctrl Pts',(-0.107121587134001,0.111178312051432,
0.409561326593314));
#16789=CARTESIAN_POINT('Ctrl Pts',(-0.0611933749717542,0.141742803557285,
0.406914996714211));
#16790=CARTESIAN_POINT('Ctrl Pts',(-0.0129361277491455,0.146018041789781,
0.40426866683511));
#16791=CARTESIAN_POINT('Ctrl Pts',(0.0353211194734639,0.150293280022276,
0.401622336956008));
#16792=CARTESIAN_POINT('Ctrl Pts',(0.0859074017564354,0.128279264981412,
0.398976007076906));
#16793=CARTESIAN_POINT('Ctrl Pts',(0.115668581836909,0.0900521576926538,
0.396329677197804));
#16794=CARTESIAN_POINT('Ctrl Pts',(0.145429761917382,0.0518250504038959,
0.393683347318702));
#16795=CARTESIAN_POINT('Ctrl Pts',(0.154365839795359,-0.0026151491327561,
0.3910370174396));
#16796=CARTESIAN_POINT('Ctrl Pts',(0.138386632036901,-0.0483503050946702,
0.388390687560498));
#16797=CARTESIAN_POINT('Ctrl Pts',(0.122407424278443,-0.094085461056585,
0.385744357681396));
#16798=CARTESIAN_POINT('Ctrl Pts',(0.0815129308835505,-0.131115573443762,
0.383098027802294));
#16799=CARTESIAN_POINT('Ctrl Pts',(0.0344212048624006,-0.142491377230642,
0.380451697923192));
#16800=CARTESIAN_POINT('Ctrl Pts',(-0.0126705211587486,-0.153867181017521,
0.37780536804409));
#16801=CARTESIAN_POINT('Ctrl Pts',(-0.0659594798061549,-0.139588676204105,
0.375159038164988));
#16802=CARTESIAN_POINT('Ctrl Pts',(-0.101054476324393,-0.106191359083811,
0.372512708285887));
#16803=CARTESIAN_POINT('Ctrl Pts',(-0.129554902927378,-0.0790696072742943,
0.370363640385355));
#16804=CARTESIAN_POINT('Ctrl Pts',(-0.146056480184715,-0.0393390709180539,
0.368214572484823));
#16805=CARTESIAN_POINT('Ctrl Pts',(-0.146416087288192,0.000126442170093593,
0.366065504584291));
#16806=CARTESIAN_POINT('Ctrl Pts',(-0.146408012399712,0.000128195943346294,
0.358934495415711));
#16807=CARTESIAN_POINT('Ctrl Pts',(-0.146048368712081,-0.0390859965171687,
0.361069574826434));
#16808=CARTESIAN_POINT('Ctrl Pts',(-0.1297855810823,-0.0785633296797545,
0.363204654237157));
#16809=CARTESIAN_POINT('Ctrl Pts',(-0.101613371150224,-0.105657280969165,
0.36533973364788));
#16810=CARTESIAN_POINT('Ctrl Pts',(-0.066681270335132,-0.139252396162569,
0.36798712302214));
#16811=CARTESIAN_POINT('Ctrl Pts',(-0.0134387509101597,-0.153808392568477,
0.370634512396399));
#16812=CARTESIAN_POINT('Ctrl Pts',(0.0337263783221333,-0.142657876135818,
0.373281901770659));
#16813=CARTESIAN_POINT('Ctrl Pts',(0.0808915075544263,-0.13150735970316,
0.375929291144919));
#16814=CARTESIAN_POINT('Ctrl Pts',(0.12197924659404,-0.0946503304319347,
0.378576680519179));
#16815=CARTESIAN_POINT('Ctrl Pts',(0.138169300408926,-0.0489692009616054,
0.38122406989344));
#16816=CARTESIAN_POINT('Ctrl Pts',(0.154359354223812,-0.00328807149127619,
0.3838714592677));
#16817=CARTESIAN_POINT('Ctrl Pts',(0.14565172281397,0.0512171581781573,
0.38651884864196));
#16818=CARTESIAN_POINT('Ctrl Pts',(0.11603494864959,0.0895802930905963,
0.38916623801622));
#16819=CARTESIAN_POINT('Ctrl Pts',(0.0864181744852101,0.127943428003035,
0.39181362739048));
#16820=CARTESIAN_POINT('Ctrl Pts',(0.0358922575662923,0.15016446815848,
0.394461016764739));
#16821=CARTESIAN_POINT('Ctrl Pts',(-0.0123993367959677,0.146065035738641,
0.397108406138999));
#16822=CARTESIAN_POINT('Ctrl Pts',(-0.0606909311582276,0.141965603318802,
0.399755795513259));
#16823=CARTESIAN_POINT('Ctrl Pts',(-0.106748202963829,0.111545698323679,
0.40240318488752));
#16824=CARTESIAN_POINT('Ctrl Pts',(-0.129474555904152,0.0687391998188283,
0.40505057426178));
#16825=CARTESIAN_POINT('Ctrl Pts',(-0.140588317483115,0.0478057390183907,
0.406345214646423));
#16826=CARTESIAN_POINT('Ctrl Pts',(-0.146122589096428,0.0239100770892618,
0.407639855031067));
#16827=CARTESIAN_POINT('Ctrl Pts',(-0.146109756335714,8.81622270207575E-6,
0.40893449541571));
#16828=CARTESIAN_POINT('Origin',(0.,0.,0.));
#16829=CARTESIAN_POINT('',(-0.146374718215768,-0.000132229735885947,0.466065504584291));
#16830=CARTESIAN_POINT('',(-0.146375609273197,-0.000132432188538665,0.458934495415711));
#16831=CARTESIAN_POINT('',(-0.14635,-1.79227059055215E-17,0.));
#16832=CARTESIAN_POINT('Ctrl Pts',(-0.146374718215768,-0.000132229735885947,
0.466065504584291));
#16833=CARTESIAN_POINT('Ctrl Pts',(-0.146022504084922,0.0379941335185874,
0.46399086782161));
#16834=CARTESIAN_POINT('Ctrl Pts',(-0.130761950520226,0.0763703265456945,
0.46191623105893));
#16835=CARTESIAN_POINT('Ctrl Pts',(-0.103994021541854,0.103314352404769,
0.45984159429625));
#16836=CARTESIAN_POINT('Ctrl Pts',(-0.0698498419286355,0.137683154682254,
0.457195264417148));
#16837=CARTESIAN_POINT('Ctrl Pts',(-0.0169824611430249,0.153451124186949,
0.454548934538046));
#16838=CARTESIAN_POINT('Ctrl Pts',(0.030409888879481,0.143401013202843,
0.451902604658944));
#16839=CARTESIAN_POINT('Ctrl Pts',(0.0778022389019875,0.133350902218736,
0.449256274779842));
#16840=CARTESIAN_POINT('Ctrl Pts',(0.119719558161389,0.0974827107458278,
0.44660994490074));
#16841=CARTESIAN_POINT('Ctrl Pts',(0.136975630157447,0.0522138743269898,
0.443963615021638));
#16842=CARTESIAN_POINT('Ctrl Pts',(0.154231702153504,0.00694503790815254,
0.441317285142536));
#16843=CARTESIAN_POINT('Ctrl Pts',(0.146826526886218,-0.0477244434566137,
0.438670955263434));
#16844=CARTESIAN_POINT('Ctrl Pts',(0.118149569579287,-0.0867714880447125,
0.436024625384332));
#16845=CARTESIAN_POINT('Ctrl Pts',(0.0894726122723542,-0.125818532632812,
0.43337829550523));
#16846=CARTESIAN_POINT('Ctrl Pts',(0.0395238729257754,-0.149243140444243,
0.430731965626129));
#16847=CARTESIAN_POINT('Ctrl Pts',(-0.00883432462988853,-0.146323499949933,
0.428085635747027));
#16848=CARTESIAN_POINT('Ctrl Pts',(-0.0571925221855517,-0.143403859455623,
0.425439305867925));
#16849=CARTESIAN_POINT('Ctrl Pts',(-0.1039601779503,-0.114139970655572,
0.422792975988823));
#16850=CARTESIAN_POINT('Ctrl Pts',(-0.127731000096207,-0.0719263758553634,
0.420146646109721));
#16851=CARTESIAN_POINT('Ctrl Pts',(-0.139950702323481,-0.0502259249733931,
0.418786265601244));
#16852=CARTESIAN_POINT('Ctrl Pts',(-0.146093241566443,-0.0251033736724598,
0.417425885092767));
#16853=CARTESIAN_POINT('Ctrl Pts',(-0.146110491840834,1.12683595067248E-5,
0.416065504584291));
#16854=CARTESIAN_POINT('Ctrl Pts',(-0.146109756335714,8.81622270207575E-6,
0.40893449541571));
#16855=CARTESIAN_POINT('Ctrl Pts',(-0.146096347589706,-0.0249652282079418,
0.410287244405327));
#16856=CARTESIAN_POINT('Ctrl Pts',(-0.140026707259891,-0.049945385460595,
0.411639993394943));
#16857=CARTESIAN_POINT('Ctrl Pts',(-0.127937780377622,-0.0715588049813403,
0.412992742384559));
#16858=CARTESIAN_POINT('Ctrl Pts',(-0.104279217835726,-0.113857219262079,
0.415640131758819));
#16859=CARTESIAN_POINT('Ctrl Pts',(-0.0575666586768896,-0.14326095580898,
0.41828752113308));
#16860=CARTESIAN_POINT('Ctrl Pts',(-0.00919685447762893,-0.146301592903247,
0.42093491050734));
#16861=CARTESIAN_POINT('Ctrl Pts',(0.039172949721632,-0.149342229997515,
0.4235822998816));
#16862=CARTESIAN_POINT('Ctrl Pts',(0.089199998961318,-0.126019767639148,
0.426229689255859));
#16863=CARTESIAN_POINT('Ctrl Pts',(0.117969334952632,-0.0870170915920772,
0.428877078630119));
#16864=CARTESIAN_POINT('Ctrl Pts',(0.146738670943946,-0.0480144155450057,
0.431524468004379));
#16865=CARTESIAN_POINT('Ctrl Pts',(0.154250293686888,0.00666847419077017,
0.43417185737864));
#16866=CARTESIAN_POINT('Ctrl Pts',(0.137063494116028,0.051984005222912,
0.4368192467529));
#16867=CARTESIAN_POINT('Ctrl Pts',(0.119876694545168,0.0972995362550541,
0.43946663612716));
#16868=CARTESIAN_POINT('Ctrl Pts',(0.0779914726605056,0.133247708583562,
0.442114025501419));
#16869=CARTESIAN_POINT('Ctrl Pts',(0.0305934116013849,0.143362412733947,
0.444761414875679));
#16870=CARTESIAN_POINT('Ctrl Pts',(-0.0168046494577345,0.153477116884331,
0.447408804249939));
#16871=CARTESIAN_POINT('Ctrl Pts',(-0.0697155496913122,0.137758352856595,
0.4500561936242));
#16872=CARTESIAN_POINT('Ctrl Pts',(-0.103903378920715,0.103406122000434,
0.45270358299846));
#16873=CARTESIAN_POINT('Ctrl Pts',(-0.130724942802416,0.0764555792150183,
0.45478055380421));
#16874=CARTESIAN_POINT('Ctrl Pts',(-0.146022533856355,0.0380362146017157,
0.45685752460996));
#16875=CARTESIAN_POINT('Ctrl Pts',(-0.146375609273197,-0.000132432188538665,
0.458934495415711));
#16876=CARTESIAN_POINT('Origin',(0.,0.,0.));
#16877=CARTESIAN_POINT('',(-0.146548608312775,6.99729089778146E-5,0.516065504584291));
#16878=CARTESIAN_POINT('',(-0.146550766805835,6.86360251013434E-5,0.508934495415711));
#16879=CARTESIAN_POINT('',(-0.14635,-1.79227059055215E-17,0.));
#16880=CARTESIAN_POINT('Ctrl Pts',(-0.146548608312775,6.99729089778146E-5,
0.516065504584291));
#16881=CARTESIAN_POINT('Ctrl Pts',(-0.146572081366671,0.00404546554386884,
0.515848510308657));
#16882=CARTESIAN_POINT('Ctrl Pts',(-0.146424333269732,0.00801918670503405,
0.515631516033023));
#16883=CARTESIAN_POINT('Ctrl Pts',(-0.146099725131082,0.0119784074854107,
0.51541452175739));
#16884=CARTESIAN_POINT('Ctrl Pts',(-0.142141002193345,0.06026265009261,
0.512768191878288));
#16885=CARTESIAN_POINT('Ctrl Pts',(-0.111878319621163,0.106390286678145,
0.510121861999186));
#16886=CARTESIAN_POINT('Ctrl Pts',(-0.069163383343408,0.129247972261684,
0.507475532120084));
#16887=CARTESIAN_POINT('Ctrl Pts',(-0.0264484470656534,0.152105657845224,
0.504829202240982));
#16888=CARTESIAN_POINT('Ctrl Pts',(0.0287187429176733,0.151693392426768,
0.50218287236188));
#16889=CARTESIAN_POINT('Ctrl Pts',(0.07108729581893,0.128199876374419,0.499536542482778));
#16890=CARTESIAN_POINT('Ctrl Pts',(0.113455848720186,0.10470636032207,0.496890212603677));
#16891=CARTESIAN_POINT('Ctrl Pts',(0.143025764539373,0.0581315936358261,
0.494243882724575));
#16892=CARTESIAN_POINT('Ctrl Pts',(0.146262427589597,0.00979357977770552,
0.491597552845473));
#16893=CARTESIAN_POINT('Ctrl Pts',(0.149499090639821,-0.0385444340804161,
0.488951222966371));
#16894=CARTESIAN_POINT('Ctrl Pts',(0.126402500921083,-0.0886456951104151,
0.486304893087269));
#16895=CARTESIAN_POINT('Ctrl Pts',(0.087544330920799,-0.117578067907642,
0.483658563208167));
#16896=CARTESIAN_POINT('Ctrl Pts',(0.0486861609205161,-0.146510440704867,
0.481012233329065));
#16897=CARTESIAN_POINT('Ctrl Pts',(-0.00593358936131212,-0.154273925269321,
0.478365903449963));
#16898=CARTESIAN_POINT('Ctrl Pts',(-0.0513146009011563,-0.137315052574797,
0.475719573570861));
#16899=CARTESIAN_POINT('Ctrl Pts',(-0.0966956124410008,-0.120356179880273,
0.473073243691759));
#16900=CARTESIAN_POINT('Ctrl Pts',(-0.132837885238862,-0.078674949926771,
0.470426913812657));
#16901=CARTESIAN_POINT('Ctrl Pts',(-0.14319853241738,-0.0313495174248821,
0.467780583933555));
#16902=CARTESIAN_POINT('Ctrl Pts',(-0.145436768368387,-0.0211256884885646,
0.467208890817134));
#16903=CARTESIAN_POINT('Ctrl Pts',(-0.146471775395962,-0.0106384445195334,
0.466637197700712));
#16904=CARTESIAN_POINT('Ctrl Pts',(-0.146374718215768,-0.000132229735885947,
0.466065504584291));
#16905=CARTESIAN_POINT('Ctrl Pts',(-0.146375609273197,-0.000132432188538665,
0.458934495415711));
#16906=CARTESIAN_POINT('Ctrl Pts',(-0.146472577787773,-0.0106150565970108,
0.45950491398422));
#16907=CARTESIAN_POINT('Ctrl Pts',(-0.145442327125792,-0.021078770125739,
0.46007533255273));
#16908=CARTESIAN_POINT('Ctrl Pts',(-0.143213999951756,-0.0312807998000163,
0.460645751121239));
#16909=CARTESIAN_POINT('Ctrl Pts',(-0.132872033528166,-0.0786297930597184,
0.463293140495499));
#16910=CARTESIAN_POINT('Ctrl Pts',(-0.0967233424557573,-0.120342081894533,
0.465940529869759));
#16911=CARTESIAN_POINT('Ctrl Pts',(-0.0513258840937604,-0.13731129538499,
0.46858791924402));
#16912=CARTESIAN_POINT('Ctrl Pts',(-0.00592842573176499,-0.154280508875447,
0.47123530861828));
#16913=CARTESIAN_POINT('Ctrl Pts',(0.0487177999198187,-0.146506647021548,
0.47388269799254));
#16914=CARTESIAN_POINT('Ctrl Pts',(0.0875820145025328,-0.117550537871965,
0.476530087366799));
#16915=CARTESIAN_POINT('Ctrl Pts',(0.126446229085248,-0.0885944287223814,
0.47917747674106));
#16916=CARTESIAN_POINT('Ctrl Pts',(0.149528432599094,-0.0384560722771122,
0.481824866115319));
#16917=CARTESIAN_POINT('Ctrl Pts',(0.146255790172295,0.0098985887573764,
0.484472255489579));
#16918=CARTESIAN_POINT('Ctrl Pts',(0.142983147745498,0.0582532497918637,
0.487119644863839));
#16919=CARTESIAN_POINT('Ctrl Pts',(0.113355659378058,0.10482421541557,0.4897670342381));
#16920=CARTESIAN_POINT('Ctrl Pts',(0.0709442366160257,0.128279591164298,
0.49241442361236));
#16921=CARTESIAN_POINT('Ctrl Pts',(0.0285328138539934,0.151734966913027,
0.49506181298662));
#16922=CARTESIAN_POINT('Ctrl Pts',(-0.0266625433026316,0.152074752786777,
0.497709202360879));
#16923=CARTESIAN_POINT('Ctrl Pts',(-0.0693595260588707,0.129143309401606,
0.500356591735139));
#16924=CARTESIAN_POINT('Ctrl Pts',(-0.11205650881511,0.106211866016435,
0.503003981109399));
#16925=CARTESIAN_POINT('Ctrl Pts',(-0.142255117170964,0.060009193372344,
0.505651370483659));
#16926=CARTESIAN_POINT('Ctrl Pts',(-0.146122837288996,0.0116984888307781,
0.50829875985792));
#16927=CARTESIAN_POINT('Ctrl Pts',(-0.146432431239741,0.00783142983325791,
0.508510671710517));
#16928=CARTESIAN_POINT('Ctrl Pts',(-0.14657331536999,0.00395086404934249,
0.508722583563114));
#16929=CARTESIAN_POINT('Ctrl Pts',(-0.146550766805835,6.86360251013434E-5,
0.508934495415711));
#16930=CARTESIAN_POINT('Origin',(0.,0.,0.));
#16931=CARTESIAN_POINT('',(-0.146165204287215,8.83645032875094E-5,0.566065504584291));
#16932=CARTESIAN_POINT('',(-0.146168951232552,9.12430751481418E-5,0.558934495415711));
#16933=CARTESIAN_POINT('',(-0.14635,-1.79227059055215E-17,0.));
#16934=CARTESIAN_POINT('Ctrl Pts',(-0.146165204287215,8.83645032875094E-5,
0.566065504584291));
#16935=CARTESIAN_POINT('Ctrl Pts',(-0.146267412293664,0.0186373661349918,
0.565059822916602));
#16936=CARTESIAN_POINT('Ctrl Pts',(-0.142994166834961,0.0371516370495788,
0.564054141248913));
#16937=CARTESIAN_POINT('Ctrl Pts',(-0.136179985035193,0.0542551712289143,
0.563048459581224));
#16938=CARTESIAN_POINT('Ctrl Pts',(-0.118249288396568,0.0992610562830057,
0.560402129702122));
#16939=CARTESIAN_POINT('Ctrl Pts',(-0.0758005933416487,0.134498778989873,
0.55775579982302));
#16940=CARTESIAN_POINT('Ctrl Pts',(-0.0282633354322908,0.143839479279877,
0.555109469943918));
#16941=CARTESIAN_POINT('Ctrl Pts',(0.0192739224770691,0.153180179569881,
0.552463140064816));
#16942=CARTESIAN_POINT('Ctrl Pts',(0.0718997432408687,0.136623857443018,
0.549816810185715));
#16943=CARTESIAN_POINT('Ctrl Pts',(0.105526460745998,0.101748602013432,
0.547170480306613));
#16944=CARTESIAN_POINT('Ctrl Pts',(0.139153178251127,0.0668733465838454,
0.544524150427511));
#16945=CARTESIAN_POINT('Ctrl Pts',(0.153780792497586,0.0136791578515372,
0.541877820548409));
#16946=CARTESIAN_POINT('Ctrl Pts',(0.142714014311998,-0.0334861471092027,
0.539231490669307));
#16947=CARTESIAN_POINT('Ctrl Pts',(0.13164723612641,-0.0806514520699426,
0.536585160790205));
#16948=CARTESIAN_POINT('Ctrl Pts',(0.0948860655087725,-0.121787873259113,
0.533938830911103));
#16949=CARTESIAN_POINT('Ctrl Pts',(0.0492566686055307,-0.138066623508903,
0.531292501032001));
#16950=CARTESIAN_POINT('Ctrl Pts',(0.00362727170228945,-0.154345373758693,
0.528646171152899));
#16951=CARTESIAN_POINT('Ctrl Pts',(-0.050870351486557,-0.145766453069103,
0.525999841273797));
#16952=CARTESIAN_POINT('Ctrl Pts',(-0.089291781429334,-0.116256568409877,
0.523353511394695));
#16953=CARTESIAN_POINT('Ctrl Pts',(-0.124562723435938,-0.0891664410515947,
0.520924175791227));
#16954=CARTESIAN_POINT('Ctrl Pts',(-0.146285818313441,-0.0444372186796531,
0.518494840187759));
#16955=CARTESIAN_POINT('Ctrl Pts',(-0.146548608312775,6.99729089778146E-5,
0.516065504584291));
#16956=CARTESIAN_POINT('Ctrl Pts',(-0.146550766805835,6.86360251013434E-5,
0.508934495415711));
#16957=CARTESIAN_POINT('Ctrl Pts',(-0.146291618860727,-0.0445493453248537,
0.511369972937373));
#16958=CARTESIAN_POINT('Ctrl Pts',(-0.124445252016267,-0.0893868858389474,
0.513805450459036));
#16959=CARTESIAN_POINT('Ctrl Pts',(-0.0890226177929609,-0.116463349340462,
0.516240927980699));
#16960=CARTESIAN_POINT('Ctrl Pts',(-0.0505178462986829,-0.145895746531099,
0.518888317354959));
#16961=CARTESIAN_POINT('Ctrl Pts',(0.00402852857008221,-0.154341804473332,
0.52153570672922));
#16962=CARTESIAN_POINT('Ctrl Pts',(0.0496314652424392,-0.137932794781367,
0.52418309610348));
#16963=CARTESIAN_POINT('Ctrl Pts',(0.0952344019147948,-0.121523785089403,
0.52683048547774));
#16964=CARTESIAN_POINT('Ctrl Pts',(0.131893900390741,-0.0802597077632436,
0.529477874851999));
#16965=CARTESIAN_POINT('Ctrl Pts',(0.14281802728161,-0.0330416298281342,
0.532125264226259));
#16966=CARTESIAN_POINT('Ctrl Pts',(0.153742154172479,0.0141764481069759,
0.53477265360052));
#16967=CARTESIAN_POINT('Ctrl Pts',(0.138930909478268,0.0673485266510362,
0.53742004297478));
#16968=CARTESIAN_POINT('Ctrl Pts',(0.105168604077417,0.102119062543277,
0.54006743234904));
#16969=CARTESIAN_POINT('Ctrl Pts',(0.0714062986765666,0.136889598435517,
0.5427148217233));
#16970=CARTESIAN_POINT('Ctrl Pts',(0.018692932569077,0.153258591675938,
0.545362211097559));
#16971=CARTESIAN_POINT('Ctrl Pts',(-0.0288260648428939,0.143728202535144,
0.548009600471819));
#16972=CARTESIAN_POINT('Ctrl Pts',(-0.0763450622548654,0.13419781339435,
0.550656989846079));
#16973=CARTESIAN_POINT('Ctrl Pts',(-0.118669690971318,0.0987680418723385,
0.55330437922034));
#16974=CARTESIAN_POINT('Ctrl Pts',(-0.136413096952957,0.0536675432455532,
0.5559517685946));
#16975=CARTESIAN_POINT('Ctrl Pts',(-0.143076734904351,0.036729792140314,
0.556946010868304));
#16976=CARTESIAN_POINT('Ctrl Pts',(-0.146273385252938,0.0184280612467595,
0.557940253142007));
#16977=CARTESIAN_POINT('Ctrl Pts',(-0.146168951232552,9.12430751481418E-5,
0.558934495415711));
#16978=CARTESIAN_POINT('Origin',(0.,0.,0.));
#16979=CARTESIAN_POINT('',(-0.146227179098081,-0.000117664897458569,0.616065504584291));
#16980=CARTESIAN_POINT('',(-0.146218520919543,-0.000115076211918358,0.608934495415711));
#16981=CARTESIAN_POINT('',(-0.14635,-1.79227059055215E-17,0.));
#16982=CARTESIAN_POINT('Ctrl Pts',(-0.146227179098081,-0.000117664897458569,
0.616065504584291));
#16983=CARTESIAN_POINT('Ctrl Pts',(-0.145977603365176,0.0329427899635141,
0.614271135524546));
#16984=CARTESIAN_POINT('Ctrl Pts',(-0.134874795495675,0.0661550248562671,
0.612476766464802));
#16985=CARTESIAN_POINT('Ctrl Pts',(-0.114309815624116,0.091770790457776,
0.610682397405058));
#16986=CARTESIAN_POINT('Ctrl Pts',(-0.0839806476072558,0.129548841477563,
0.608036067525956));
#16987=CARTESIAN_POINT('Ctrl Pts',(-0.0330710111925292,0.150804375664025,
0.605389737646855));
#16988=CARTESIAN_POINT('Ctrl Pts',(0.0151169520838501,0.145808400611758,
0.602743407767753));
#16989=CARTESIAN_POINT('Ctrl Pts',(0.0633049153602295,0.140812425559491,
0.600097077888651));
#16990=CARTESIAN_POINT('Ctrl Pts',(0.108771205498262,0.109564941268491,
0.597450748009549));
#16991=CARTESIAN_POINT('Ctrl Pts',(0.130705186191441,0.0663684129079872,
0.594804418130447));
#16992=CARTESIAN_POINT('Ctrl Pts',(0.152639166884621,0.023171884547483,
0.592158088251345));
#16993=CARTESIAN_POINT('Ctrl Pts',(0.151040838132949,-0.0319736878825246,
0.589511758372243));
#16994=CARTESIAN_POINT('Ctrl Pts',(0.126641780152193,-0.0738273082886534,
0.586865428493141));
#16995=CARTESIAN_POINT('Ctrl Pts',(0.102242722171437,-0.115680928694782,
0.584219098614039));
#16996=CARTESIAN_POINT('Ctrl Pts',(0.0550429349615966,-0.14424259707703,
0.581572768734937));
#16997=CARTESIAN_POINT('Ctrl Pts',(0.00664650371163741,-0.14643918846291,
0.578926438855836));
#16998=CARTESIAN_POINT('Ctrl Pts',(-0.0417499275383225,-0.148635779848789,
0.576280108976733));
#16999=CARTESIAN_POINT('Ctrl Pts',(-0.0913430028284016,-0.1244672942383,
0.573633779097631));
#17000=CARTESIAN_POINT('Ctrl Pts',(-0.119433191362276,-0.0849960277323969,
0.570987449218529));
#17001=CARTESIAN_POINT('Ctrl Pts',(-0.136848298201485,-0.0605249807527623,
0.569346801007117));
#17002=CARTESIAN_POINT('Ctrl Pts',(-0.145998464265635,-0.0301720919893573,
0.567706152795704));
#17003=CARTESIAN_POINT('Ctrl Pts',(-0.146165204287215,8.83645032875094E-5,
0.566065504584291));
#17004=CARTESIAN_POINT('Ctrl Pts',(-0.146168951232552,9.12430751481418E-5,
0.558934495415711));
#17005=CARTESIAN_POINT('Ctrl Pts',(-0.145995306636495,-0.0303977620653178,
0.560587642516267));
#17006=CARTESIAN_POINT('Ctrl Pts',(-0.136695352934655,-0.0609837708898569,
0.562240789616823));
#17007=CARTESIAN_POINT('Ctrl Pts',(-0.119031718004195,-0.0855580991331628,
0.563893936717379));
#17008=CARTESIAN_POINT('Ctrl Pts',(-0.090744749826965,-0.124912017153538,
0.566541326091639));
#17009=CARTESIAN_POINT('Ctrl Pts',(-0.0410086302256792,-0.148848627462727,
0.5691887154659));
#17010=CARTESIAN_POINT('Ctrl Pts',(0.00739494322942312,-0.146403732988417,
0.57183610484016));
#17011=CARTESIAN_POINT('Ctrl Pts',(0.0557985166845234,-0.143958838514108,
0.57448349421442));
#17012=CARTESIAN_POINT('Ctrl Pts',(0.10286954399344,-0.1151324392563,0.57713088358868));
#17013=CARTESIAN_POINT('Ctrl Pts',(0.127047076753504,-0.0731285067993286,
0.579778272962939));
#17014=CARTESIAN_POINT('Ctrl Pts',(0.151224609513568,-0.031124574342357,
0.5824256623372));
#17015=CARTESIAN_POINT('Ctrl Pts',(0.15250864772478,0.0240568913137802,
0.58507305171146));
#17016=CARTESIAN_POINT('Ctrl Pts',(0.130311035929276,0.0671399443948921,
0.58772044108572));
#17017=CARTESIAN_POINT('Ctrl Pts',(0.108113424133771,0.110222997476006,
0.59036783045998));
#17018=CARTESIAN_POINT('Ctrl Pts',(0.0624341623315493,0.141207637982093,
0.593015219834239));
#17019=CARTESIAN_POINT('Ctrl Pts',(0.0141966988324609,0.145901308974836,
0.595662609208499));
#17020=CARTESIAN_POINT('Ctrl Pts',(-0.0340407646666261,0.150594979967579,
0.598309998582759));
#17021=CARTESIAN_POINT('Ctrl Pts',(-0.0848364298625779,0.128997681446978,
0.60095738795702));
#17022=CARTESIAN_POINT('Ctrl Pts',(-0.114923272877171,0.091002085522857,
0.60360477733128));
#17023=CARTESIAN_POINT('Ctrl Pts',(-0.135113526827902,0.0655045372973676,
0.60538135002609));
#17024=CARTESIAN_POINT('Ctrl Pts',(-0.14597798884013,0.0326223532682757,
0.6071579227209));
#17025=CARTESIAN_POINT('Ctrl Pts',(-0.146218520919543,-0.000115076211918358,
0.608934495415711));
#17026=CARTESIAN_POINT('Origin',(0.,0.,0.));
#17027=CARTESIAN_POINT('',(-0.146586033401767,-2.15382961294558E-5,0.66606550458429));
#17028=CARTESIAN_POINT('',(-0.146582846697157,-3.00215943766004E-5,0.65893449541571));
#17029=CARTESIAN_POINT('',(-0.14635,-1.79227059055215E-17,0.));
#17030=CARTESIAN_POINT('Ctrl Pts',(-0.146586033401767,-2.15382961294558E-5,
0.66606550458429));
#17031=CARTESIAN_POINT('Ctrl Pts',(-0.146488810225965,0.0472697707580183,
0.663482448132491));
#17032=CARTESIAN_POINT('Ctrl Pts',(-0.121516563758978,0.0946492637554097,
0.660899391680692));
#17033=CARTESIAN_POINT('Ctrl Pts',(-0.0824084263440199,0.121233094478226,
0.658316335228893));
#17034=CARTESIAN_POINT('Ctrl Pts',(-0.0423423130056393,0.148468111155377,
0.655670005349791));
#17035=CARTESIAN_POINT('Ctrl Pts',(0.0125607065496858,0.153876184485078,
0.653023675470689));
#17036=CARTESIAN_POINT('Ctrl Pts',(0.0571706564953393,0.134981954220393,
0.650377345591587));
#17037=CARTESIAN_POINT('Ctrl Pts',(0.101780606440992,0.116087723955709,
0.647731015712485));
#17038=CARTESIAN_POINT('Ctrl Pts',(0.136097486776972,0.0728911900966409,
0.645084685833384));
#17039=CARTESIAN_POINT('Ctrl Pts',(0.144413921474191,0.0251640857912735,
0.642438355954282));
#17040=CARTESIAN_POINT('Ctrl Pts',(0.152730356171409,-0.0225630185140953,
0.63979202607518));
#17041=CARTESIAN_POINT('Ctrl Pts',(0.135046345229863,-0.0748206932657649,
0.637145696196077));
#17042=CARTESIAN_POINT('Ctrl Pts',(0.0994561386758346,-0.10768977857233,
0.634499366316975));
#17043=CARTESIAN_POINT('Ctrl Pts',(0.0638659321218069,-0.140558863878895,
0.631853036437873));
#17044=CARTESIAN_POINT('Ctrl Pts',(0.0103695299552984,-0.154039359740357,
0.629206706558772));
#17045=CARTESIAN_POINT('Ctrl Pts',(-0.0365469229059137,-0.141961031115491,
0.62656037667967));
#17046=CARTESIAN_POINT('Ctrl Pts',(-0.0834633757671259,-0.129882702490626,
0.623914046800568));
#17047=CARTESIAN_POINT('Ctrl Pts',(-0.123799879323041,-0.0922455493794331,
0.621267716921466));
#17048=CARTESIAN_POINT('Ctrl Pts',(-0.139093781291504,-0.0462766888972804,
0.618621387042364));
#17049=CARTESIAN_POINT('Ctrl Pts',(-0.14401750805555,-0.0314774500153124,
0.617769426223006));
#17050=CARTESIAN_POINT('Ctrl Pts',(-0.14634567687575,-0.0158146654998378,
0.616917465403648));
#17051=CARTESIAN_POINT('Ctrl Pts',(-0.146227179098081,-0.000117664897458569,
0.616065504584291));
#17052=CARTESIAN_POINT('Ctrl Pts',(-0.146218520919543,-0.000115076211918358,
0.608934495415711));
#17053=CARTESIAN_POINT('Ctrl Pts',(-0.1463364217222,-0.0161618722236638,
0.60980531209516));
#17054=CARTESIAN_POINT('Ctrl Pts',(-0.143901781624712,-0.032173889023867,
0.61067612877461));
#17055=CARTESIAN_POINT('Ctrl Pts',(-0.138761720114909,-0.0472643972675185,
0.611546945454059));
#17056=CARTESIAN_POINT('Ctrl Pts',(-0.123135303504819,-0.0931413908061287,
0.614194334828319));
#17057=CARTESIAN_POINT('Ctrl Pts',(-0.0825044494514074,-0.130501484555709,
0.616841724202579));
#17058=CARTESIAN_POINT('Ctrl Pts',(-0.0354801761942514,-0.142231836504824,
0.619489113576839));
#17059=CARTESIAN_POINT('Ctrl Pts',(0.0115440970629072,-0.15396218845394,
0.6221365029511));
#17060=CARTESIAN_POINT('Ctrl Pts',(0.0649617895238099,-0.140062798602586,
0.624783892325359));
#17061=CARTESIAN_POINT('Ctrl Pts',(0.100304854137336,-0.106900301471969,
0.627431281699619));
#17062=CARTESIAN_POINT('Ctrl Pts',(0.135647918750861,-0.0737378043413545,
0.630078671073879));
#17063=CARTESIAN_POINT('Ctrl Pts',(0.15291635551701,-0.0213121999314781,
0.63272606044814));
#17064=CARTESIAN_POINT('Ctrl Pts',(0.144200333369931,0.026362891994447,
0.6353734498224));
#17065=CARTESIAN_POINT('Ctrl Pts',(0.135484311222852,0.0740379839203748,
0.63802083919666));
#17066=CARTESIAN_POINT('Ctrl Pts',(0.100783830162543,0.11696256336235,0.640668228570919));
#17067=CARTESIAN_POINT('Ctrl Pts',(0.055993492972559,0.135474968031154,
0.643315617945179));
#17068=CARTESIAN_POINT('Ctrl Pts',(0.0112031557825773,0.153987372699956,
0.64596300731944));
#17069=CARTESIAN_POINT('Ctrl Pts',(-0.04367703753708,0.148087602595587,
0.6486103966937));
#17070=CARTESIAN_POINT('Ctrl Pts',(-0.0835091394177698,0.120478055479053,
0.65125778606796));
#17071=CARTESIAN_POINT('Ctrl Pts',(-0.122009894390588,0.0937913289882395,
0.653816689183877));
#17072=CARTESIAN_POINT('Ctrl Pts',(-0.146451680634158,0.0468218259492564,
0.656375592299793));
#17073=CARTESIAN_POINT('Ctrl Pts',(-0.146582846697157,-3.00215943766004E-5,
0.65893449541571));
#17074=CARTESIAN_POINT('Origin',(0.,0.,0.));
#17075=CARTESIAN_POINT('',(-0.146290249280603,0.000131112932912382,0.716065504584291));
#17076=CARTESIAN_POINT('',(-0.146307221518699,0.000133045872591754,0.708934495415711));
#17077=CARTESIAN_POINT('',(-0.14635,-1.79227059055215E-17,0.));
#17078=CARTESIAN_POINT('Ctrl Pts',(-0.146290249280603,0.000131112932912382,
0.716065504584291));
#17079=CARTESIAN_POINT('Ctrl Pts',(-0.146406294125046,0.0134819654399978,
0.715340090619538));
#17080=CARTESIAN_POINT('Ctrl Pts',(-0.144729088574721,0.0268041890186768,
0.714614676654786));
#17081=CARTESIAN_POINT('Ctrl Pts',(-0.141142411757643,0.0395908011096033,
0.713889262690033));
#17082=CARTESIAN_POINT('Ctrl Pts',(-0.128058117149462,0.0862367098911347,
0.711242932810931));
#17083=CARTESIAN_POINT('Ctrl Pts',(-0.0895623832093418,0.125754646095387,
0.708596602931829));
#17084=CARTESIAN_POINT('Ctrl Pts',(-0.0432753130058998,0.140056628595385,
0.705950273052727));
#17085=CARTESIAN_POINT('Ctrl Pts',(0.00301175719754219,0.154358611095384,
0.703303943173625));
#17086=CARTESIAN_POINT('Ctrl Pts',(0.0570901636643063,0.143444639891129,
0.700657613294523));
#17087=CARTESIAN_POINT('Ctrl Pts',(0.0942073689518517,0.11231021130972,
0.698011283415421));
#17088=CARTESIAN_POINT('Ctrl Pts',(0.131324574239397,0.0811757827283121,
0.695364953536319));
#17089=CARTESIAN_POINT('Ctrl Pts',(0.151480578347723,0.0298208967697505,
0.692718623657217));
#17090=CARTESIAN_POINT('Ctrl Pts',(0.145449661086834,-0.0182485073085286,
0.690072293778115));
#17091=CARTESIAN_POINT('Ctrl Pts',(0.139418743825945,-0.0663179113868083,
0.687425963899014));
#17092=CARTESIAN_POINT('Ctrl Pts',(0.107200905195838,-0.111101833584806,
0.684779634019911));
#17093=CARTESIAN_POINT('Ctrl Pts',(0.0635427568131047,-0.132101968137704,
0.68213330414081));
#17094=CARTESIAN_POINT('Ctrl Pts',(0.0198846084303716,-0.153102102690602,
0.679486974261708));
#17095=CARTESIAN_POINT('Ctrl Pts',(-0.0352138497049885,-0.150318449598402,
0.676840644382606));
#17096=CARTESIAN_POINT('Ctrl Pts',(-0.0765331864534889,-0.125025130675956,
0.674194314503504));
#17097=CARTESIAN_POINT('Ctrl Pts',(-0.117852523201989,-0.0997318117535095,
0.671547984624402));
#17098=CARTESIAN_POINT('Ctrl Pts',(-0.14539273856363,-0.0519288270008166,
0.6689016547453));
#17099=CARTESIAN_POINT('Ctrl Pts',(-0.146548242683733,-0.00349635461217019,
0.666255324866198));
#17100=CARTESIAN_POINT('Ctrl Pts',(-0.146575870647472,-0.00233834005587287,
0.666192051438896));
#17101=CARTESIAN_POINT('Ctrl Pts',(-0.146588414938392,-0.00117996563262623,
0.666128778011593));
#17102=CARTESIAN_POINT('Ctrl Pts',(-0.146586033401767,-2.15382961294558E-5,
0.66606550458429));
#17103=CARTESIAN_POINT('Ctrl Pts',(-0.146582846697157,-3.00215943766004E-5,
0.65893449541571));
#17104=CARTESIAN_POINT('Ctrl Pts',(-0.146587382388275,-0.00165014728799839,
0.659022981674053));
#17105=CARTESIAN_POINT('Ctrl Pts',(-0.146562848415234,-0.00327013229389975,
0.659111467932396));
#17106=CARTESIAN_POINT('Ctrl Pts',(-0.146508820881567,-0.00488913307276392,
0.659199954190739));
#17107=CARTESIAN_POINT('Ctrl Pts',(-0.144892390022949,-0.0533274503793473,
0.661847343564999));
#17108=CARTESIAN_POINT('Ctrl Pts',(-0.116875517863988,-0.100884760863813,
0.66449473293926));
#17109=CARTESIAN_POINT('Ctrl Pts',(-0.0752913709948059,-0.125777373450206,
0.66714212231352));
#17110=CARTESIAN_POINT('Ctrl Pts',(-0.0337072241256252,-0.150669986036599,
0.66978951168778));
#17111=CARTESIAN_POINT('Ctrl Pts',(0.021444197453776,-0.15289790072492,
0.672436901062039));
#17112=CARTESIAN_POINT('Ctrl Pts',(0.0649007096996251,-0.131440618146733,
0.675084290436299));
#17113=CARTESIAN_POINT('Ctrl Pts',(0.108357221945475,-0.109983335568545,
0.677731679810559));
#17114=CARTESIAN_POINT('Ctrl Pts',(0.140118824857774,-0.0648408557238465,
0.68037906918482));
#17115=CARTESIAN_POINT('Ctrl Pts',(0.145637072805965,-0.0166907532130915,
0.68302645855908));
#17116=CARTESIAN_POINT('Ctrl Pts',(0.151155320754156,0.031459349297663,
0.68567384793334));
#17117=CARTESIAN_POINT('Ctrl Pts',(0.130430213738242,0.0826170744744734,
0.688321237307599));
#17118=CARTESIAN_POINT('Ctrl Pts',(0.0929549153570804,0.113349556369966,
0.690968626681859));
#17119=CARTESIAN_POINT('Ctrl Pts',(0.0554796169759186,0.14408203826546,
0.693616016056119));
#17120=CARTESIAN_POINT('Ctrl Pts',(0.00125412722950909,0.154389276879634,
0.69626340543038));
#17121=CARTESIAN_POINT('Ctrl Pts',(-0.0448834941801804,0.139550027475769,
0.69891079480464));
#17122=CARTESIAN_POINT('Ctrl Pts',(-0.0910211155898686,0.124710778071904,
0.7015581841789));
#17123=CARTESIAN_POINT('Ctrl Pts',(-0.129070868662838,0.0847250406500019,
0.704205573553159));
#17124=CARTESIAN_POINT('Ctrl Pts',(-0.141604011991841,0.0379083368947344,
0.706852962927419));
#17125=CARTESIAN_POINT('Ctrl Pts',(-0.144888775625201,0.0256383259412015,
0.707546807090183));
#17126=CARTESIAN_POINT('Ctrl Pts',(-0.146420824649375,0.0128991016161637,
0.708240651252947));
#17127=CARTESIAN_POINT('Ctrl Pts',(-0.146307221518699,0.000133045872591754,
0.708934495415711));
#17128=CARTESIAN_POINT('Origin',(0.,0.,0.));
#17129=CARTESIAN_POINT('',(-0.1461301977291,-5.61458017395017E-5,0.766065504584291));
#17130=CARTESIAN_POINT('',(-0.14612241379348,-4.54149644099216E-5,0.758934495415711));
#17131=CARTESIAN_POINT('',(-0.14635,-1.79227059055215E-17,0.));
#17132=CARTESIAN_POINT('Ctrl Pts',(-0.1461301977291,-5.61458017395017E-5,
0.766065504584291));
#17133=CARTESIAN_POINT('Ctrl Pts',(-0.14603380141711,0.0278870014676159,
0.764551403227483));
#17134=CARTESIAN_POINT('Ctrl Pts',(-0.138327245009168,0.0558793842949389,
0.763037301870675));
#17135=CARTESIAN_POINT('Ctrl Pts',(-0.123350675409043,0.079203679241543,
0.761523200513867));
#17136=CARTESIAN_POINT('Ctrl Pts',(-0.0971747899961838,0.119969628197767,
0.758876870634766));
#17137=CARTESIAN_POINT('Ctrl Pts',(-0.048790709571801,0.146475657227381,
0.756230540755664));
#17138=CARTESIAN_POINT('Ctrl Pts',(-0.000344588961360588,0.146589539830481,
0.753584210876561));
#17139=CARTESIAN_POINT('Ctrl Pts',(0.0481015316490792,0.14670342243358,
0.750937880997459));
#17140=CARTESIAN_POINT('Ctrl Pts',(0.0966096924455767,0.120425158610167,
0.748291551118357));
#17141=CARTESIAN_POINT('Ctrl Pts',(0.122976945064223,0.0797827231418903,
0.745645221239255));
#17142=CARTESIAN_POINT('Ctrl Pts',(0.149344197682869,0.0391402876736125,
0.742998891360154));
#17143=CARTESIAN_POINT('Ctrl Pts',(0.153570542123663,-0.01586631943953,
0.740352561481052));
#17144=CARTESIAN_POINT('Ctrl Pts',(0.133721514043982,-0.0600597087159893,
0.73770623160195));
#17145=CARTESIAN_POINT('Ctrl Pts',(0.113872485964301,-0.104253097992448,
0.735059901722848));
#17146=CARTESIAN_POINT('Ctrl Pts',(0.0699480853641458,-0.137633269432224,
0.732413571843746));
#17147=CARTESIAN_POINT('Ctrl Pts',(0.0220532014503509,-0.144921593405036,
0.729767241964644));
#17148=CARTESIAN_POINT('Ctrl Pts',(-0.0258416824634434,-0.152209917377848,
0.727120912085542));
#17149=CARTESIAN_POINT('Ctrl Pts',(-0.0777070496908773,-0.133406393883698,
0.724474582206441));
#17150=CARTESIAN_POINT('Ctrl Pts',(-0.109803305666473,-0.0971176914572187,
0.721828252327339));
#17151=CARTESIAN_POINT('Ctrl Pts',(-0.133101311474982,-0.0707764758164216,
0.71990733641299));
#17152=CARTESIAN_POINT('Ctrl Pts',(-0.14598295937539,-0.0352223077304616,
0.71798642049864));
#17153=CARTESIAN_POINT('Ctrl Pts',(-0.146290249280603,0.000131112932912382,
0.716065504584291));
#17154=CARTESIAN_POINT('Ctrl Pts',(-0.146307221518699,0.000133045872591754,
0.708934495415711));
#17155=CARTESIAN_POINT('Ctrl Pts',(-0.145987367488279,-0.0358102803178394,
0.710888040627207));
#17156=CARTESIAN_POINT('Ctrl Pts',(-0.132622002370819,-0.0719663061161047,
0.712841585838703));
#17157=CARTESIAN_POINT('Ctrl Pts',(-0.1086007072861,-0.0984612847532928,
0.7147951310502));
#17158=CARTESIAN_POINT('Ctrl Pts',(-0.0760477256663158,-0.134366532557423,
0.71744252042446));
#17159=CARTESIAN_POINT('Ctrl Pts',(-0.0239252288417074,-0.152529358077047,
0.720089909798719));
#17160=CARTESIAN_POINT('Ctrl Pts',(0.0238920022682765,-0.144630254255197,
0.722737299172979));
#17161=CARTESIAN_POINT('Ctrl Pts',(0.071709233378259,-0.136731150433346,
0.725384688547239));
#17162=CARTESIAN_POINT('Ctrl Pts',(0.115221198773618,-0.102770117270024,
0.7280320779215));
#17163=CARTESIAN_POINT('Ctrl Pts',(0.134497183226257,-0.058303052428779,
0.730679467295759));
#17164=CARTESIAN_POINT('Ctrl Pts',(0.153773167678896,-0.0138359875875333,
0.733326856670019));
#17165=CARTESIAN_POINT('Ctrl Pts',(0.148813171188813,0.0411371089316358,
0.735974246044279));
#17166=CARTESIAN_POINT('Ctrl Pts',(0.121889126928366,0.0814357351225549,
0.738621635418539));
#17167=CARTESIAN_POINT('Ctrl Pts',(0.0949650826679194,0.121734361313473,
0.741269024792799));
#17168=CARTESIAN_POINT('Ctrl Pts',(0.0460769906371109,0.147358517176143,
0.74391641416706));
#17169=CARTESIAN_POINT('Ctrl Pts',(-0.00238189178169058,0.146571023090686,
0.74656380354132));
#17170=CARTESIAN_POINT('Ctrl Pts',(-0.0508407742004934,0.14578352900523,
0.74921119291558));
#17171=CARTESIAN_POINT('Ctrl Pts',(-0.0988704470072894,0.118584384971644,
0.751858582289839));
#17172=CARTESIAN_POINT('Ctrl Pts',(-0.124470852918682,0.0774321960944291,
0.754505971664099));
#17173=CARTESIAN_POINT('Ctrl Pts',(-0.138745545153454,0.0544858868428234,
0.75598214624797));
#17174=CARTESIAN_POINT('Ctrl Pts',(-0.146046671909043,0.027201385339783,
0.757458320831841));
#17175=CARTESIAN_POINT('Ctrl Pts',(-0.14612241379348,-4.54149644099216E-5,
0.758934495415711));
#17176=CARTESIAN_POINT('Origin',(0.,0.,0.));
#17177=CARTESIAN_POINT('',(-0.146495788566881,-0.000101744904923998,0.816065504584291));
#17178=CARTESIAN_POINT('',(-0.146473871348434,-0.000110945968026819,0.808934495415711));
#17179=CARTESIAN_POINT('',(-0.14635,-1.79227059055215E-17,0.));
#17180=CARTESIAN_POINT('Ctrl Pts',(-0.146495788566881,-0.000101744904923998,
0.816065504584291));
#17181=CARTESIAN_POINT('Ctrl Pts',(-0.14616118452328,0.0421270051992108,
0.813762715835428));
#17182=CARTESIAN_POINT('Ctrl Pts',(-0.126905337350145,0.0846218946815527,
0.811459927086565));
#17183=CARTESIAN_POINT('Ctrl Pts',(-0.0947343415465314,0.111866064832055,
0.809157138337701));
#17184=CARTESIAN_POINT('Ctrl Pts',(-0.0577639214515077,0.143174651664521,
0.806510808458599));
#17185=CARTESIAN_POINT('Ctrl Pts',(-0.00373742343573488,0.154342745753647,
0.803864478579497));
#17186=CARTESIAN_POINT('Ctrl Pts',(0.0426163743729279,0.140258534729872,
0.801218148700395));
#17187=CARTESIAN_POINT('Ctrl Pts',(0.0889701721815907,0.126174323706097,
0.798571818821294));
#17188=CARTESIAN_POINT('Ctrl Pts',(0.127651269783143,0.0868378075694234,
0.795925488942192));
#17189=CARTESIAN_POINT('Ctrl Pts',(0.140954720244851,0.040253928627653,
0.79327915906309));
#17190=CARTESIAN_POINT('Ctrl Pts',(0.154258170706558,-0.00632995031411615,
0.790632829183988));
#17191=CARTESIAN_POINT('Ctrl Pts',(0.14218397402842,-0.060161192060982,
0.787986499304886));
#17192=CARTESIAN_POINT('Ctrl Pts',(0.110258679990485,-0.0966003903512828,
0.785340169425784));
#17193=CARTESIAN_POINT('Ctrl Pts',(0.0783333859525485,-0.133039588641585,
0.782693839546682));
#17194=CARTESIAN_POINT('Ctrl Pts',(0.0265569945548152,-0.152086743475322,
0.780047509667581));
#17195=CARTESIAN_POINT('Ctrl Pts',(-0.021371625274328,-0.14502367242074,
0.777401179788479));
#17196=CARTESIAN_POINT('Ctrl Pts',(-0.0693002451034712,-0.137960601366157,
0.774754849909377));
#17197=CARTESIAN_POINT('Ctrl Pts',(-0.113381093364023,-0.104787304423254,
0.772108520030274));
#17198=CARTESIAN_POINT('Ctrl Pts',(-0.133437672293631,-0.0606877215103841,
0.769462190151172));
#17199=CARTESIAN_POINT('Ctrl Pts',(-0.1420188514214,-0.0418197768941368,
0.768329961628878));
#17200=CARTESIAN_POINT('Ctrl Pts',(-0.146202281842484,-0.0209517273285418,
0.767197733106584));
#17201=CARTESIAN_POINT('Ctrl Pts',(-0.1461301977291,-5.61458017395017E-5,
0.766065504584291));
#17202=CARTESIAN_POINT('Ctrl Pts',(-0.14612241379348,-4.54149644099216E-5,
0.758934495415711));
#17203=CARTESIAN_POINT('Ctrl Pts',(-0.146182508321779,-0.0216633562673834,
0.760105710206101));
#17204=CARTESIAN_POINT('Ctrl Pts',(-0.141694203021096,-0.0432575645610501,
0.76127692499649));
#17205=CARTESIAN_POINT('Ctrl Pts',(-0.132531725405586,-0.0626424774360703,
0.76244813978688));
#17206=CARTESIAN_POINT('Ctrl Pts',(-0.111821052965107,-0.106459728368519,
0.76509552916114));
#17207=CARTESIAN_POINT('Ctrl Pts',(-0.067228569068158,-0.138988996512573,
0.767742918535399));
#17208=CARTESIAN_POINT('Ctrl Pts',(-0.0191799219195066,-0.145330206128911,
0.770390307909659));
#17209=CARTESIAN_POINT('Ctrl Pts',(0.0288687252291434,-0.151671415745249,
0.773037697283919));
#17210=CARTESIAN_POINT('Ctrl Pts',(0.080373535629496,-0.131824566833873,
0.77568508665818));
#17211=CARTESIAN_POINT('Ctrl Pts',(0.111742660473083,-0.0948805356683208,
0.77833247603244));
#17212=CARTESIAN_POINT('Ctrl Pts',(0.14311178531667,-0.0579365045027684,
0.7809798654067));
#17213=CARTESIAN_POINT('Ctrl Pts',(0.154345224603492,-0.00389529108304171,
0.783627254780959));
#17214=CARTESIAN_POINT('Ctrl Pts',(0.140297486112651,0.0424894529122293,
0.786274644155219));
#17215=CARTESIAN_POINT('Ctrl Pts',(0.126249747621811,0.0888741969075009,
0.788922033529479));
#17216=CARTESIAN_POINT('Ctrl Pts',(0.0869208313533056,0.127602471478316,
0.79156942290374));
#17217=CARTESIAN_POINT('Ctrl Pts',(0.0403254011646538,0.140934737517831,
0.794216812278));
#17218=CARTESIAN_POINT('Ctrl Pts',(-0.00627002902399674,0.154267003557346,
0.79686420165226));
#17219=CARTESIAN_POINT('Ctrl Pts',(-0.0601319731327944,0.142203261065564,
0.799511591026519));
#17220=CARTESIAN_POINT('Ctrl Pts',(-0.0965888940360299,0.110269323781398,
0.802158980400779));
#17221=CARTESIAN_POINT('Ctrl Pts',(-0.127690529151203,0.0830262752573849,
0.804417485405756));
#17222=CARTESIAN_POINT('Ctrl Pts',(-0.146124951115714,0.0413218847513699,
0.806675990410734));
#17223=CARTESIAN_POINT('Ctrl Pts',(-0.146473871348434,-0.000110945968026819,
0.808934495415711));
#17224=CARTESIAN_POINT('Origin',(0.,0.,0.));
#17225=CARTESIAN_POINT('',(-0.146444331750498,0.000119944961782359,0.866065504584291));
#17226=CARTESIAN_POINT('',(-0.146471560192382,0.00011177640072981,0.858934495415711));
#17227=CARTESIAN_POINT('',(-0.14635,-1.79227059055215E-17,0.));
#17228=CARTESIAN_POINT('Ctrl Pts',(-0.146444331750498,0.000119944961782359,
0.866065504584291));
#17229=CARTESIAN_POINT('Ctrl Pts',(-0.146516681599632,0.00829054204730037,
0.865620358322474));
#17230=CARTESIAN_POINT('Ctrl Pts',(-0.145891801779796,0.0164500693154795,
0.865175212060658));
#17231=CARTESIAN_POINT('Ctrl Pts',(-0.14453063157077,0.0244848619971339,
0.864730065798841));
#17232=CARTESIAN_POINT('Ctrl Pts',(-0.136438672357208,0.0722505376181754,
0.862083735919739));
#17233=CARTESIAN_POINT('Ctrl Pts',(-0.102325254887189,0.115607931012472,
0.859437406040638));
#17234=CARTESIAN_POINT('Ctrl Pts',(-0.0578046270350215,0.134711681091902,
0.856791076161536));
#17235=CARTESIAN_POINT('Ctrl Pts',(-0.0132839991828526,0.153815431171333,
0.854144746282434));
#17236=CARTESIAN_POINT('Ctrl Pts',(0.0416438390514653,0.148665537935894,
0.851498416403331));
#17237=CARTESIAN_POINT('Ctrl Pts',(0.081837551941475,0.121619188541491,
0.848852086524229));
#17238=CARTESIAN_POINT('Ctrl Pts',(0.122031264831484,0.0945728391470885,
0.846205756645128));
#17239=CARTESIAN_POINT('Ctrl Pts',(0.147490852377186,0.0456300335937214,
0.843559426766026));
#17240=CARTESIAN_POINT('Ctrl Pts',(0.146563060809277,-0.0028073360113171,
0.840913096886925));
#17241=CARTESIAN_POINT('Ctrl Pts',(0.145635269241369,-0.0512447056163556,
0.838266767007823));
#17242=CARTESIAN_POINT('Ctrl Pts',(0.118320098559852,-0.0991766392730661,
0.835620437128721));
#17243=CARTESIAN_POINT('Ctrl Pts',(0.0771201321287374,-0.124663936845065,
0.832974107249619));
#17244=CARTESIAN_POINT('Ctrl Pts',(0.035920165697623,-0.150151234417064,
0.830327777370517));
#17245=CARTESIAN_POINT('Ctrl Pts',(-0.0191645964830881,-0.153193895904352,
0.827681447491415));
#17246=CARTESIAN_POINT('Ctrl Pts',(-0.0629209921278279,-0.132399247274726,
0.825035117612313));
#17247=CARTESIAN_POINT('Ctrl Pts',(-0.106677387772568,-0.111604598645101,
0.822388787733211));
#17248=CARTESIAN_POINT('Ctrl Pts',(-0.139105416881337,-0.0669726398985626,
0.819742457854109));
#17249=CARTESIAN_POINT('Ctrl Pts',(-0.145362260348583,-0.0189321207373897,
0.817096127975007));
#17250=CARTESIAN_POINT('Ctrl Pts',(-0.146174510965348,-0.0126955988357878,
0.816752586844768));
#17251=CARTESIAN_POINT('Ctrl Pts',(-0.146545706411658,-0.00640163348415362,
0.81640904571453));
#17252=CARTESIAN_POINT('Ctrl Pts',(-0.146495788566881,-0.000101744904923998,
0.816065504584291));
#17253=CARTESIAN_POINT('Ctrl Pts',(-0.146473871348434,-0.000110945968026819,
0.808934495415711));
#17254=CARTESIAN_POINT('Ctrl Pts',(-0.146533950748007,-0.00724512552769256,
0.809323379784994));
#17255=CARTESIAN_POINT('Ctrl Pts',(-0.146057826922151,-0.0143712538186879,
0.809712264154277));
#17256=CARTESIAN_POINT('Ctrl Pts',(-0.145017839345608,-0.0214141189368497,
0.81010114852356));
#17257=CARTESIAN_POINT('Ctrl Pts',(-0.137937966054276,-0.0693594922943736,
0.81274853789782));
#17258=CARTESIAN_POINT('Ctrl Pts',(-0.104726321773939,-0.113446106932874,
0.81539592727208));
#17259=CARTESIAN_POINT('Ctrl Pts',(-0.0605955455659204,-0.133480028752914,
0.818043316646339));
#17260=CARTESIAN_POINT('Ctrl Pts',(-0.0164647693578984,-0.153513950572954,
0.820690706020599));
#17261=CARTESIAN_POINT('Ctrl Pts',(0.0385851387778066,-0.149495179574532,
0.823338095394859));
#17262=CARTESIAN_POINT('Ctrl Pts',(0.0793384931690736,-0.12326451930694,
0.825985484769119));
#17263=CARTESIAN_POINT('Ctrl Pts',(0.120091847560339,-0.0970338590393495,
0.828632874143379));
#17264=CARTESIAN_POINT('Ctrl Pts',(0.146548648207165,-0.0485913095025905,
0.83128026351764));
#17265=CARTESIAN_POINT('Ctrl Pts',(0.146590321408106,-0.000126046730599388,
0.833927652891899));
#17266=CARTESIAN_POINT('Ctrl Pts',(0.146631994609047,0.0483392160413931,
0.836575042266159));
#17267=CARTESIAN_POINT('Ctrl Pts',(0.120258540364101,0.0968271920486179,
0.839222431640419));
#17268=CARTESIAN_POINT('Ctrl Pts',(0.0795503554414038,0.123127897600245,
0.841869821014679));
#17269=CARTESIAN_POINT('Ctrl Pts',(0.0388421705187073,0.149428603151872,
0.844517210388939));
#17270=CARTESIAN_POINT('Ctrl Pts',(-0.0162007450817403,0.153542038247903,
0.8471645997632));
#17271=CARTESIAN_POINT('Ctrl Pts',(-0.0603659086281491,0.133584038319734,
0.84981198913746));
#17272=CARTESIAN_POINT('Ctrl Pts',(-0.104531072174558,0.113626038391565,
0.85245937851172));
#17273=CARTESIAN_POINT('Ctrl Pts',(-0.137818483666928,0.0695966034391962,
0.855106767885979));
#17274=CARTESIAN_POINT('Ctrl Pts',(-0.144980798768897,0.0216634763286692,
0.857754157260239));
#17275=CARTESIAN_POINT('Ctrl Pts',(-0.146045237806912,0.0145398171508471,
0.858147603312063));
#17276=CARTESIAN_POINT('Ctrl Pts',(-0.146532654486068,0.00732993751956911,
0.858541049363887));
#17277=CARTESIAN_POINT('Ctrl Pts',(-0.146471560192382,0.00011177640072981,
0.858934495415711));
#17278=CARTESIAN_POINT('Origin',(0.,0.,0.));
#17279=CARTESIAN_POINT('',(-0.146114231148477,2.69008449349656E-5,0.916065504584291));
#17280=CARTESIAN_POINT('',(-0.146121644853617,4.41067432152685E-5,0.908934495415711));
#17281=CARTESIAN_POINT('',(-0.14635,-1.79227059055215E-17,0.));
#17282=CARTESIAN_POINT('Ctrl Pts',(-0.146114231148477,2.69008449349656E-5,
0.916065504584291));
#17283=CARTESIAN_POINT('Ctrl Pts',(-0.146151635159142,0.0228038459942234,
0.914831670930419));
#17284=CARTESIAN_POINT('Ctrl Pts',(-0.141147538069067,0.0455652341090756,
0.913597837276548));
#17285=CARTESIAN_POINT('Ctrl Pts',(-0.131015765267123,0.0657531838068269,
0.912364003622676));
#17286=CARTESIAN_POINT('Ctrl Pts',(-0.109285110563454,0.109052354902802,
0.909717673743574));
#17287=CARTESIAN_POINT('Ctrl Pts',(-0.0639662294071284,0.140513248471977,
0.907071343864472));
#17288=CARTESIAN_POINT('Ctrl Pts',(-0.015802286694576,0.145735718560985,
0.90442501398537));
#17289=CARTESIAN_POINT('Ctrl Pts',(0.0323616560179757,0.150958188649994,
0.901778684106268));
#17290=CARTESIAN_POINT('Ctrl Pts',(0.0833706602867547,0.129942235258839,
0.899132354227166));
#17291=CARTESIAN_POINT('Ctrl Pts',(0.113877102345416,0.0923071908936453,
0.896486024348064));
#17292=CARTESIAN_POINT('Ctrl Pts',(0.144383544404078,0.0546721465284523,
0.893839694468962));
#17293=CARTESIAN_POINT('Ctrl Pts',(0.15438742425262,0.000418011189221586,
0.891193364589861));
#17294=CARTESIAN_POINT('Ctrl Pts',(0.139309808695705,-0.0456222438118789,
0.888547034710759));
#17295=CARTESIAN_POINT('Ctrl Pts',(0.124232193138789,-0.0916624988129813,
0.885900704831657));
#17296=CARTESIAN_POINT('Ctrl Pts',(0.0840730821764119,-0.129488873475953,
0.883254374952555));
#17297=CARTESIAN_POINT('Ctrl Pts',(0.0372139327097935,-0.141787641004198,
0.880608045073453));
#17298=CARTESIAN_POINT('Ctrl Pts',(-0.00964521675682358,-0.154086408532443,
0.877961715194351));
#17299=CARTESIAN_POINT('Ctrl Pts',(-0.0632044047276821,-0.140857568925962,
0.875315385315249));
#17300=CARTESIAN_POINT('Ctrl Pts',(-0.0989487482345592,-0.108156170198829,
0.872669055436147));
#17301=CARTESIAN_POINT('Ctrl Pts',(-0.128680439645858,-0.0809555616469925,
0.870467871818862));
#17302=CARTESIAN_POINT('Ctrl Pts',(-0.146086572253705,-0.0402824710322022,
0.868266688201576));
#17303=CARTESIAN_POINT('Ctrl Pts',(-0.146444331750498,0.000119944961782359,
0.866065504584291));
#17304=CARTESIAN_POINT('Ctrl Pts',(-0.146471560192382,0.00011177640072981,
0.858934495415711));
#17305=CARTESIAN_POINT('Ctrl Pts',(-0.146121567926216,-0.0412390669452651,
0.861188438738147));
#17306=CARTESIAN_POINT('Ctrl Pts',(-0.127770397964496,-0.0828616943330661,
0.863442382060584));
#17307=CARTESIAN_POINT('Ctrl Pts',(-0.096778382793969,-0.110103055552942,
0.86569632538302));
#17308=CARTESIAN_POINT('Ctrl Pts',(-0.0603764330055066,-0.142099641055337,
0.86834371475728));
#17309=CARTESIAN_POINT('Ctrl Pts',(-0.00653531471701479,-0.154255992791443,
0.870991104131539));
#17310=CARTESIAN_POINT('Ctrl Pts',(0.040082974241256,-0.14100387723139,
0.873638493505799));
#17311=CARTESIAN_POINT('Ctrl Pts',(0.0867012631995282,-0.127751761671338,
0.876285882880059));
#17312=CARTESIAN_POINT('Ctrl Pts',(0.12609672282758,-0.0890911788151255,
0.878933272254319));
#17313=CARTESIAN_POINT('Ctrl Pts',(0.140224208991091,-0.042730661487191,
0.88158066162858));
#17314=CARTESIAN_POINT('Ctrl Pts',(0.154351695154603,0.00362985584074295,
0.88422805100284));
#17315=CARTESIAN_POINT('Ctrl Pts',(0.143211207853577,0.057690307640398,
0.886875440377099));
#17316=CARTESIAN_POINT('Ctrl Pts',(0.111905662524754,0.09468823006692,0.889522829751359));
#17317=CARTESIAN_POINT('Ctrl Pts',(0.0806001171959318,0.131686152493442,
0.892170219125619));
#17318=CARTESIAN_POINT('Ctrl Pts',(0.0291295138393125,0.15162154554683,
0.894817608499879));
#17319=CARTESIAN_POINT('Ctrl Pts',(-0.0189299673197759,0.145362975188259,
0.897464997874139));
#17320=CARTESIAN_POINT('Ctrl Pts',(-0.0669894484788628,0.139104404829688,
0.9001123872484));
#17321=CARTESIAN_POINT('Ctrl Pts',(-0.11163780744042,0.10665187105916,0.902759776622659));
#17322=CARTESIAN_POINT('Ctrl Pts',(-0.132423802349956,0.0628703013313112,
0.905407165996919));
#17323=CARTESIAN_POINT('Ctrl Pts',(-0.141655418982822,0.043425734493323,
0.90658294246985));
#17324=CARTESIAN_POINT('Ctrl Pts',(-0.146180218154578,0.0217465313827003,
0.907758718942781));
#17325=CARTESIAN_POINT('Ctrl Pts',(-0.146121644853617,4.41067432152685E-5,
0.908934495415711));
#17326=CARTESIAN_POINT('Origin',(0.,0.,0.));
#17327=CARTESIAN_POINT('',(-0.146345621585321,-0.000133809880645736,0.966065504584291));
#17328=CARTESIAN_POINT('',(-0.146309694201085,-0.000133223314395004,0.958934495415711));
#17329=CARTESIAN_POINT('',(-0.14635,-1.79227059055215E-17,0.));
#17330=CARTESIAN_POINT('Ctrl Pts',(-0.146345621585321,-0.000133809880645736,
0.966065504584291));
#17331=CARTESIAN_POINT('Ctrl Pts',(-0.146004672532387,0.0370537288701324,
0.964042983538364));
#17332=CARTESIAN_POINT('Ctrl Pts',(-0.131578083002406,0.0744765756810296,
0.962020462492437));
#17333=CARTESIAN_POINT('Ctrl Pts',(-0.106003654037246,0.101251356830495,
0.959997941446511));
#17334=CARTESIAN_POINT('Ctrl Pts',(-0.0725412702228666,0.136284319036219,
0.957351611567409));
#17335=CARTESIAN_POINT('Ctrl Pts',(-0.0199938687303381,0.153087872523943,
0.954705281688306));
#17336=CARTESIAN_POINT('Ctrl Pts',(0.0275867780614433,0.143970766496025,
0.952058951809204));
#17337=CARTESIAN_POINT('Ctrl Pts',(0.0751674248532248,0.134853660468108,
0.949412621930102));
#17338=CARTESIAN_POINT('Ctrl Pts',(0.11778131694426,0.0998158949245492,
0.946766292051));
#17339=CARTESIAN_POINT('Ctrl Pts',(0.135923405490256,0.0548948063954655,
0.944119962171899));
#17340=CARTESIAN_POINT('Ctrl Pts',(0.154065494036253,0.0099737178663825,
0.941473632292797));
#17341=CARTESIAN_POINT('Ctrl Pts',(0.147735779037212,-0.0448306936482241,
0.938827302413695));
#17342=CARTESIAN_POINT('Ctrl Pts',(0.119831470632095,-0.0844335867733556,
0.936180972534593));
#17343=CARTESIAN_POINT('Ctrl Pts',(0.0919271622269763,-0.124036479898489,
0.933534642655491));
#17344=CARTESIAN_POINT('Ctrl Pts',(0.0424482604157787,-0.148437854634144,
0.93088831277639));
#17345=CARTESIAN_POINT('Ctrl Pts',(-0.00595796300272124,-0.146468817862788,
0.928241982897288));
#17346=CARTESIAN_POINT('Ctrl Pts',(-0.0543641864212212,-0.144499781091432,
0.925595653018186));
#17347=CARTESIAN_POINT('Ctrl Pts',(-0.101697731447024,-0.116160332813065,
0.922949323139084));
#17348=CARTESIAN_POINT('Ctrl Pts',(-0.126293289834417,-0.0744218843624929,
0.920302993259982));
#17349=CARTESIAN_POINT('Ctrl Pts',(-0.139421333187579,-0.052143709087005,
0.918890497034752));
#17350=CARTESIAN_POINT('Ctrl Pts',(-0.146071410932229,-0.0260482098028304,
0.917478000809521));
#17351=CARTESIAN_POINT('Ctrl Pts',(-0.146114231148477,2.69008449349656E-5,
0.916065504584291));
#17352=CARTESIAN_POINT('Ctrl Pts',(-0.146121644853617,4.41067432152685E-5,
0.908934495415711));
#17353=CARTESIAN_POINT('Ctrl Pts',(-0.146048333958771,-0.027118852224649,
0.910406108317041));
#17354=CARTESIAN_POINT('Ctrl Pts',(-0.138795050353101,-0.0543181883240968,
0.91187772121837));
#17355=CARTESIAN_POINT('Ctrl Pts',(-0.124603830013468,-0.0772180274565794,
0.9133493341197));
#17356=CARTESIAN_POINT('Ctrl Pts',(-0.0990742319099257,-0.118414180831446,
0.91599672349396));
#17357=CARTESIAN_POINT('Ctrl Pts',(-0.0510914048453256,-0.145695881896007,
0.91864411286822));
#17358=CARTESIAN_POINT('Ctrl Pts',(-0.00263394834681351,-0.146566710184873,
0.92129150224248));
#17359=CARTESIAN_POINT('Ctrl Pts',(0.0458235081516972,-0.147437538473739,
0.92393889161674));
#17360=CARTESIAN_POINT('Ctrl Pts',(0.0947555940841207,-0.121897493986912,
0.926586280990999));
#17361=CARTESIAN_POINT('Ctrl Pts',(0.121748900601314,-0.0816452290135895,
0.929233670365259));
#17362=CARTESIAN_POINT('Ctrl Pts',(0.148742207118509,-0.0413929640402651,
0.931881059739519));
#17363=CARTESIAN_POINT('Ctrl Pts',(0.153796734220472,0.0135715214195569,
0.93452844911378));
#17364=CARTESIAN_POINT('Ctrl Pts',(0.134597248858856,0.0580716696672091,
0.93717583848804));
#17365=CARTESIAN_POINT('Ctrl Pts',(0.115397763497239,0.102571817914861,
0.9398232278623));
#17366=CARTESIAN_POINT('Ctrl Pts',(0.0719442656720451,0.136607628950342,
0.942470617236559));
#17367=CARTESIAN_POINT('Ctrl Pts',(0.0241406894609324,0.144588953003544,
0.945118006610819));
#17368=CARTESIAN_POINT('Ctrl Pts',(-0.023662886750181,0.152570277056746,
0.947765395985079));
#17369=CARTESIAN_POINT('Ctrl Pts',(-0.0758165413472122,0.134497114127667,
0.950412785359339));
#17370=CARTESIAN_POINT('Ctrl Pts',(-0.108431221550465,0.0986479012011113,
0.953060174733599));
#17371=CARTESIAN_POINT('Ctrl Pts',(-0.132554242808212,0.0721325001574252,
0.955018281627637));
#17372=CARTESIAN_POINT('Ctrl Pts',(-0.145988218858404,0.0358924841874147,
0.956976388521674));
#17373=CARTESIAN_POINT('Ctrl Pts',(-0.146309694201085,-0.000133223314395004,
0.958934495415711));
#17374=CARTESIAN_POINT('Origin',(0.,0.,0.));
#17375=CARTESIAN_POINT('',(-0.146565171121453,5.44893591410845E-5,1.01606550458429));
#17376=CARTESIAN_POINT('',(-0.146582076026177,3.15354312248815E-5,1.00893449541571));
#17377=CARTESIAN_POINT('',(-0.14635,-1.79227059055215E-17,0.));
#17378=CARTESIAN_POINT('Ctrl Pts',(-0.146565171121453,5.44893591410845E-5,
1.01606550458429));
#17379=CARTESIAN_POINT('Ctrl Pts',(-0.146579596851449,0.00307427920823236,
1.01590062602541));
#17380=CARTESIAN_POINT('Ctrl Pts',(-0.146494352296349,0.00609323927190738,
1.01573574746653));
#17381=CARTESIAN_POINT('Ctrl Pts',(-0.146306854564556,0.00910583530985269,
1.01557086890765));
#17382=CARTESIAN_POINT('Ctrl Pts',(-0.143297482980539,0.0574585317612167,
1.01292453902855));
#17383=CARTESIAN_POINT('Ctrl Pts',(-0.11394685994478,0.104171803331984,
1.01027820914945));
#17384=CARTESIAN_POINT('Ctrl Pts',(-0.0716892273871119,0.127864250695428,
1.00763187927034));
#17385=CARTESIAN_POINT('Ctrl Pts',(-0.0294315948294418,0.151556698058874,
1.00498554939124));
#17386=CARTESIAN_POINT('Ctrl Pts',(0.0257330472501378,0.152228321214993,
1.00233921951214));
#17387=CARTESIAN_POINT('Ctrl Pts',(0.0685549742796134,0.129571707678744,
0.999692889633039));
#17388=CARTESIAN_POINT('Ctrl Pts',(0.111376901309088,0.106915094142495,
0.997046559753937));
#17389=CARTESIAN_POINT('Ctrl Pts',(0.141856113288459,0.0609302439138786,
0.994400229874835));
#17390=CARTESIAN_POINT('Ctrl Pts',(0.146041795372579,0.0126651464112397,
0.991753899995733));
#17391=CARTESIAN_POINT('Ctrl Pts',(0.150227477456699,-0.0355999510913994,
0.989107570116631));
#17392=CARTESIAN_POINT('Ctrl Pts',(0.128119629645567,-0.0861452958680607,
0.986461240237529));
#17393=CARTESIAN_POINT('Ctrl Pts',(0.0898373616998479,-0.115835488396583,
0.983814910358427));
#17394=CARTESIAN_POINT('Ctrl Pts',(0.051555093754129,-0.145525680925106,
0.981168580479325));
#17395=CARTESIAN_POINT('Ctrl Pts',(-0.00290159432617693,-0.154360721205491,
0.978522250600224));
#17396=CARTESIAN_POINT('Ctrl Pts',(-0.0486070196525971,-0.138296672301818,
0.975875920721122));
#17397=CARTESIAN_POINT('Ctrl Pts',(-0.0943124449790173,-0.122232623398145,
0.97322959084202));
#17398=CARTESIAN_POINT('Ctrl Pts',(-0.131266607551552,-0.081269485310415,
0.970583260962917));
#17399=CARTESIAN_POINT('Ctrl Pts',(-0.142555005769704,-0.0341567308046872,
0.967936931083816));
#17400=CARTESIAN_POINT('Ctrl Pts',(-0.145215975052668,-0.0230510282813687,
0.967313122250641));
#17401=CARTESIAN_POINT('Ctrl Pts',(-0.146450780951306,-0.0116036114945705,
0.966689313417466));
#17402=CARTESIAN_POINT('Ctrl Pts',(-0.146345621585321,-0.000133809880645736,
0.966065504584291));
#17403=CARTESIAN_POINT('Ctrl Pts',(-0.146309694201085,-0.000133223314395004,
0.958934495415711));
#17404=CARTESIAN_POINT('Ctrl Pts',(-0.146422858258782,-0.0128148032088542,
0.959623777895933));
#17405=CARTESIAN_POINT('Ctrl Pts',(-0.14491119500038,-0.0254698272036438,
0.960313060376156));
#17406=CARTESIAN_POINT('Ctrl Pts',(-0.141668994059001,-0.037664762585484,
0.961002342856379));
#17407=CARTESIAN_POINT('Ctrl Pts',(-0.129216380554811,-0.0845029505214961,
0.963649732230639));
#17408=CARTESIAN_POINT('Ctrl Pts',(-0.0912354477369537,-0.12455406346949,
0.966297121604899));
#17409=CARTESIAN_POINT('Ctrl Pts',(-0.0451234138007503,-0.1394726343957,
0.968944510979159));
#17410=CARTESIAN_POINT('Ctrl Pts',(0.00098862013545236,-0.154391205321909,
0.97159190035342));
#17411=CARTESIAN_POINT('Ctrl Pts',(0.055231755190001,-0.144177234226336,
0.974239289727679));
#17412=CARTESIAN_POINT('Ctrl Pts',(0.0927598492034174,-0.113509244531313,
0.976886679101939));
#17413=CARTESIAN_POINT('Ctrl Pts',(0.130287943216833,-0.0828412548362905,
0.979534068476199));
#17414=CARTESIAN_POINT('Ctrl Pts',(0.151100996189117,-0.0317192465418168,
0.982181457850459));
#17415=CARTESIAN_POINT('Ctrl Pts',(0.145665560755875,0.0164402745715088,
0.984828847224719));
#17416=CARTESIAN_POINT('Ctrl Pts',(0.140230125322634,0.0645997956848379,
0.987476236598979));
#17417=CARTESIAN_POINT('Ctrl Pts',(0.108546201483865,0.109796829617019,
0.990123625973239));
#17418=CARTESIAN_POINT('Ctrl Pts',(0.0651266538643092,0.131328813193254,
0.992771015347499));
#17419=CARTESIAN_POINT('Ctrl Pts',(0.0217071062447581,0.152860796769488,
0.995418404721759));
#17420=CARTESIAN_POINT('Ctrl Pts',(-0.0334480651555777,0.15072772998978,
0.998065794096019));
#17421=CARTESIAN_POINT('Ctrl Pts',(-0.0750749586823209,0.125906667008376,
1.00071318347028));
#17422=CARTESIAN_POINT('Ctrl Pts',(-0.116701852209067,0.101085604026969,
1.00336057284454));
#17423=CARTESIAN_POINT('Ctrl Pts',(-0.144800467862219,0.053576544843864,
1.0060079622188));
#17424=CARTESIAN_POINT('Ctrl Pts',(-0.146500196332402,0.00514107896046776,
1.00865535159306));
#17425=CARTESIAN_POINT('Ctrl Pts',(-0.146559936783033,0.00343871495990628,
1.00874839953394));
#17426=CARTESIAN_POINT('Ctrl Pts',(-0.146587066279139,0.00173520655478852,
1.00884144747483));
#17427=CARTESIAN_POINT('Ctrl Pts',(-0.146582076026177,3.15354312248815E-5,
1.00893449541571));
#17428=CARTESIAN_POINT('Origin',(0.,0.,0.));
#17429=CARTESIAN_POINT('',(-0.146184049129756,9.96948043307314E-5,1.06606550458429));
#17430=CARTESIAN_POINT('',(-0.146216477546812,0.000114345603752017,1.05893449541571));
#17431=CARTESIAN_POINT('',(-0.14635,-1.79227059055215E-17,0.));
#17432=CARTESIAN_POINT('Ctrl Pts',(-0.146184049129756,9.96948043307314E-5,
1.06606550458429));
#17433=CARTESIAN_POINT('Ctrl Pts',(-0.146294264763128,0.0176817746259609,
1.06511193863336));
#17434=CARTESIAN_POINT('Ctrl Pts',(-0.143360807533043,0.0352283113603788,
1.06415837268242));
#17435=CARTESIAN_POINT('Ctrl Pts',(-0.13721959397524,0.0515693218739058,
1.06320480673148));
#17436=CARTESIAN_POINT('Ctrl Pts',(-0.120176538991979,0.0969187854681546,
1.06055847685238));
#17437=CARTESIAN_POINT('Ctrl Pts',(-0.0784283132238915,0.132983650068601,
1.05791214697328));
#17438=CARTESIAN_POINT('Ctrl Pts',(-0.0310837364199337,0.143256459747686,
1.05526581709418));
#17439=CARTESIAN_POINT('Ctrl Pts',(0.0162608403840241,0.153529269426771,
1.05261948721508));
#17440=CARTESIAN_POINT('Ctrl Pts',(0.0692017682238519,0.138010024184496,
1.04997315733597));
#17441=CARTESIAN_POINT('Ctrl Pts',(0.103507151520239,0.103802126728842,
1.04732682745687));
#17442=CARTESIAN_POINT('Ctrl Pts',(0.137812534816628,0.0695942292731864,
1.04468049757777));
#17443=CARTESIAN_POINT('Ctrl Pts',(0.153482373569574,0.01669767960415,1.04203416769867));
#17444=CARTESIAN_POINT('Ctrl Pts',(0.143344336052008,-0.0306759392859165,
1.03938783781957));
#17445=CARTESIAN_POINT('Ctrl Pts',(0.133206298534443,-0.0780495581759789,
1.03674150794047));
#17446=CARTESIAN_POINT('Ctrl Pts',(0.0972603847463712,-0.119900246287072,
1.03409517806136));
#17447=CARTESIAN_POINT('Ctrl Pts',(0.0519596049571008,-0.137072285243832,
1.03144884818226));
#17448=CARTESIAN_POINT('Ctrl Pts',(0.00665882516783032,-0.154244324200591,
1.02880251830316));
#17449=CARTESIAN_POINT('Ctrl Pts',(-0.0479968206226384,-0.146737714003016,
1.02615618842406));
#17450=CARTESIAN_POINT('Ctrl Pts',(-0.0869905834517384,-0.11798834823825,
1.02350985854496));
#17451=CARTESIAN_POINT('Ctrl Pts',(-0.123554854979944,-0.0910302005802824,
1.02102840722473));
#17452=CARTESIAN_POINT('Ctrl Pts',(-0.146348061346918,-0.0453938791777224,
1.01854695590451));
#17453=CARTESIAN_POINT('Ctrl Pts',(-0.146565171121453,5.44893591410845E-5,
1.01606550458429));
#17454=CARTESIAN_POINT('Ctrl Pts',(-0.146582076026177,3.15354312248815E-5,
1.00893449541571));
#17455=CARTESIAN_POINT('Ctrl Pts',(-0.146445084172466,-0.0467374494427972,
1.01148883684909));
#17456=CARTESIAN_POINT('Ctrl Pts',(-0.122102455869861,-0.0936290599181376,
1.01404317828246));
#17457=CARTESIAN_POINT('Ctrl Pts',(-0.0837162036049941,-0.120334265578335,
1.01659751971584));
#17458=CARTESIAN_POINT('Ctrl Pts',(-0.0439316411201867,-0.14801227165006,
1.0192449090901));
#17459=CARTESIAN_POINT('Ctrl Pts',(0.0109383251366414,-0.154006411209824,
1.02189229846436));
#17460=CARTESIAN_POINT('Ctrl Pts',(0.0557604321169594,-0.135571060438576,
1.02453968783862));
#17461=CARTESIAN_POINT('Ctrl Pts',(0.100582539097277,-0.11713570966733,
1.02718707721288));
#17462=CARTESIAN_POINT('Ctrl Pts',(0.135356786801084,-0.0742708685650716,
1.02983446658714));
#17463=CARTESIAN_POINT('Ctrl Pts',(0.144154783532934,-0.0266108361928598,
1.0324818559614));
#17464=CARTESIAN_POINT('Ctrl Pts',(0.152952780264784,0.0210491961793507,
1.03512924533566));
#17465=CARTESIAN_POINT('Ctrl Pts',(0.135774526024679,0.0735044198215165,
1.03777663470992));
#17466=CARTESIAN_POINT('Ctrl Pts',(0.100488543649143,0.106727647840587,
1.04042402408418));
#17467=CARTESIAN_POINT('Ctrl Pts',(0.0652025612736062,0.139950875859659,
1.04307141345844));
#17468=CARTESIAN_POINT('Ctrl Pts',(0.0118088507626404,0.153942108255635,
1.0457188028327));
#17469=CARTESIAN_POINT('Ctrl Pts',(-0.0352355257975899,0.142292641904202,
1.04836619220696));
#17470=CARTESIAN_POINT('Ctrl Pts',(-0.0822799023578202,0.130643175552769,
1.05101358158122));
#17471=CARTESIAN_POINT('Ctrl Pts',(-0.122974944967313,0.0933530104539243,
1.05366097095548));
#17472=CARTESIAN_POINT('Ctrl Pts',(-0.138680233730631,0.0475029577050484,
1.05630836032974));
#17473=CARTESIAN_POINT('Ctrl Pts',(-0.143873300563147,0.0323423075707214,
1.05718373869173));
#17474=CARTESIAN_POINT('Ctrl Pts',(-0.146334133026589,0.0162457690968458,
1.05805911705372));
#17475=CARTESIAN_POINT('Ctrl Pts',(-0.146216477546812,0.000114345603752017,
1.05893449541571));
#17476=CARTESIAN_POINT('Origin',(0.,0.,0.));
#17477=CARTESIAN_POINT('',(-0.146204073634541,-0.000109175101205505,1.11606550458429));
#17478=CARTESIAN_POINT('',(-0.146170555016798,-9.22629125885076E-5,1.10893449541571));
#17479=CARTESIAN_POINT('',(-0.14635,-1.79227059055215E-17,0.));
#17480=CARTESIAN_POINT('Ctrl Pts',(-0.146204073634541,-0.000109175101205505,
1.11606550458429));
#17481=CARTESIAN_POINT('Ctrl Pts',(-0.145981599624502,0.032003853555373,
1.1143232512413));
#17482=CARTESIAN_POINT('Ctrl Pts',(-0.135565881201595,0.0642480963468658,
1.11258099789831));
#17483=CARTESIAN_POINT('Ctrl Pts',(-0.11609067353381,0.0895073597405865,
1.11083874455532));
#17484=CARTESIAN_POINT('Ctrl Pts',(-0.0865095427755784,0.127873963375947,
1.10819241467622));
#17485=CARTESIAN_POINT('Ctrl Pts',(-0.0360273159486943,0.150125560802435,
1.10554608479712));
#17486=CARTESIAN_POINT('Ctrl Pts',(0.0122494975033169,0.14607724579886,
1.10289975491801));
#17487=CARTESIAN_POINT('Ctrl Pts',(0.0605263109553308,0.142028930795284,
1.10025342503891));
#17488=CARTESIAN_POINT('Ctrl Pts',(0.10659771103247,0.111680703361642,1.09760709515981));
#17489=CARTESIAN_POINT('Ctrl Pts',(0.129376093089052,0.0689234246557527,
1.09496076528071));
#17490=CARTESIAN_POINT('Ctrl Pts',(0.152154475145634,0.0261661459498645,
1.09231443540161));
#17491=CARTESIAN_POINT('Ctrl Pts',(0.151639839181659,-0.0290001840282729,
1.0896681055225));
#17492=CARTESIAN_POINT('Ctrl Pts',(0.128067742174483,-0.0713250681289163,
1.0870217756434));
#17493=CARTESIAN_POINT('Ctrl Pts',(0.104495645167307,-0.11364995222956,
1.0843754457643));
#17494=CARTESIAN_POINT('Ctrl Pts',(0.0578660871169326,-0.143133390452712,
1.0817291158852));
#17495=CARTESIAN_POINT('Ctrl Pts',(0.00952215035475689,-0.146280349267719,
1.0790827860061));
#17496=CARTESIAN_POINT('Ctrl Pts',(-0.0388217864074202,-0.149427308082725,
1.07643645612699));
#17497=CARTESIAN_POINT('Ctrl Pts',(-0.0888801018813974,-0.126237787489585,
1.07379012624789));
#17498=CARTESIAN_POINT('Ctrl Pts',(-0.117740317519168,-0.0873259958989869,
1.07114379636879));
#17499=CARTESIAN_POINT('Ctrl Pts',(-0.136201180005177,-0.0624354946409797,
1.06945103244062));
#17500=CARTESIAN_POINT('Ctrl Pts',(-0.145988395071105,-0.0311118962502767,
1.06775826851246));
#17501=CARTESIAN_POINT('Ctrl Pts',(-0.146184049129756,9.96948043307314E-5,
1.06606550458429));
#17502=CARTESIAN_POINT('Ctrl Pts',(-0.146216477546812,0.000114345603752017,
1.05893449541571));
#17503=CARTESIAN_POINT('Ctrl Pts',(-0.145978309898544,-0.0325401742182177,
1.06070650642798));
#17504=CARTESIAN_POINT('Ctrl Pts',(-0.135174246449945,-0.06533764273189,
1.06247851744025));
#17505=CARTESIAN_POINT('Ctrl Pts',(-0.115079600404687,-0.0908043159161929,
1.06425052845252));
#17506=CARTESIAN_POINT('Ctrl Pts',(-0.0850581433982766,-0.128851596389654,
1.06689791782678));
#17507=CARTESIAN_POINT('Ctrl Pts',(-0.0342996944683099,-0.150536216937668,
1.06954530720104));
#17508=CARTESIAN_POINT('Ctrl Pts',(0.0139457694684962,-0.145925507476389,
1.0721926965753));
#17509=CARTESIAN_POINT('Ctrl Pts',(0.0621912334052997,-0.14131479801511,
1.07484008594956));
#17510=CARTESIAN_POINT('Ctrl Pts',(0.107923712348941,-0.110408758544542,
1.07748747532382));
#17511=CARTESIAN_POINT('Ctrl Pts',(0.1301953818052,-0.0673639426912374,
1.08013486469808));
#17512=CARTESIAN_POINT('Ctrl Pts',(0.15246705126146,-0.024319126837932,
1.08278225407234));
#17513=CARTESIAN_POINT('Ctrl Pts',(0.151277911230334,0.0308644653981125,
1.0854296434466));
#17514=CARTESIAN_POINT('Ctrl Pts',(0.127172648928576,0.0729099141598672,
1.08807703282086));
#17515=CARTESIAN_POINT('Ctrl Pts',(0.103067386626818,0.114955362921624,
1.09072442219512));
#17516=CARTESIAN_POINT('Ctrl Pts',(0.0560460020544268,0.143862668209093,
1.09337181156938));
#17517=CARTESIAN_POINT('Ctrl Pts',(0.00764670469074742,0.146390799320458,
1.09601920094364));
#17518=CARTESIAN_POINT('Ctrl Pts',(-0.0407525926729279,0.148918930431823,
1.0986665903179));
#17519=CARTESIAN_POINT('Ctrl Pts',(-0.0905298028278899,0.125067887367091,
1.10131397969216));
#17520=CARTESIAN_POINT('Ctrl Pts',(-0.11888440661962,0.0857626730052823,
1.10396136906642));
#17521=CARTESIAN_POINT('Ctrl Pts',(-0.136639133674055,0.0611510311732957,
1.10561907784952));
#17522=CARTESIAN_POINT('Ctrl Pts',(-0.145994366384503,0.0304800321277272,
1.10727678663261));
#17523=CARTESIAN_POINT('Ctrl Pts',(-0.146170555016798,-9.22629125885076E-5,
1.10893449541571));
#17524=CARTESIAN_POINT('Origin',(0.,0.,0.));
#17525=CARTESIAN_POINT('',(-0.146577386142569,-3.88073511912723E-5,1.16606550458429));
#17526=CARTESIAN_POINT('',(-0.146552328192774,-6.73160170860698E-5,1.15893449541571));
#17527=CARTESIAN_POINT('',(-0.14635,-1.79227059055215E-17,0.));
#17528=CARTESIAN_POINT('Ctrl Pts',(-0.146577386142569,-3.88073511912723E-5,
1.16606550458429));
#17529=CARTESIAN_POINT('Ctrl Pts',(-0.146413350709018,0.0463056768050285,
1.16353456384924));
#17530=CARTESIAN_POINT('Ctrl Pts',(-0.122574225104448,0.0927954474992645,
1.1610036231142));
#17531=CARTESIAN_POINT('Ctrl Pts',(-0.0847742546295189,0.119590709008994,
1.15847268237915));
#17532=CARTESIAN_POINT('Ctrl Pts',(-0.0452509303920754,0.147607604138013,
1.15582635250005));
#17533=CARTESIAN_POINT('Ctrl Pts',(0.00953524646069181,0.154093252855687,
1.15318002262095));
#17534=CARTESIAN_POINT('Ctrl Pts',(0.0545077808453859,0.136079071706768,
1.15053369274185));
#17535=CARTESIAN_POINT('Ctrl Pts',(0.0994803152300801,0.118064890557849,
1.14788736286275));
#17536=CARTESIAN_POINT('Ctrl Pts',(0.134639207146701,0.0755508795423365,
1.14524103298364));
#17537=CARTESIAN_POINT('Ctrl Pts',(0.14389167861853,0.027996370364851,1.14259470310454));
#17538=CARTESIAN_POINT('Ctrl Pts',(0.15314415009036,-0.0195581388126345,
1.13994837322544));
#17539=CARTESIAN_POINT('Ctrl Pts',(0.136490201117397,-0.0721531461520931,
1.13730204334634));
#17540=CARTESIAN_POINT('Ctrl Pts',(0.101552606157185,-0.105715089329518,
1.13465571346724));
#17541=CARTESIAN_POINT('Ctrl Pts',(0.0666150111969725,-0.139277032506943,
1.13200938358813));
#17542=CARTESIAN_POINT('Ctrl Pts',(0.0133937702495101,-0.153805911522335,
1.12936305370903));
#17543=CARTESIAN_POINT('Ctrl Pts',(-0.033750917386428,-0.142651629870951,
1.12671672382993));
#17544=CARTESIAN_POINT('Ctrl Pts',(-0.0808956050223675,-0.131497348219567,
1.12407039395083));
#17545=CARTESIAN_POINT('Ctrl Pts',(-0.121963739346782,-0.094659905901407,
1.12142406407173));
#17546=CARTESIAN_POINT('Ctrl Pts',(-0.1381577891642,-0.0490003798202082,
1.11877773419262));
#17547=CARTESIAN_POINT('Ctrl Pts',(-0.143690228857438,-0.0334015285560649,
1.11787365765651));
#17548=CARTESIAN_POINT('Ctrl Pts',(-0.146319518115206,-0.0167730178360648,
1.1169695811204));
#17549=CARTESIAN_POINT('Ctrl Pts',(-0.146204073634541,-0.000109175101205505,
1.11606550458429));
#17550=CARTESIAN_POINT('Ctrl Pts',(-0.146170555016798,-9.22629125885076E-5,
1.10893449541571));
#17551=CARTESIAN_POINT('Ctrl Pts',(-0.146275742653821,-0.0183444476975235,
1.10992417600687));
#17552=CARTESIAN_POINT('Ctrl Pts',(-0.143109248288425,-0.0365614514641733,
1.11091385659804));
#17553=CARTESIAN_POINT('Ctrl Pts',(-0.136505188007283,-0.0534328725168923,
1.1119035371892));
#17554=CARTESIAN_POINT('Ctrl Pts',(-0.118839368174718,-0.0985638180183679,
1.11455092656346));
#17555=CARTESIAN_POINT('Ctrl Pts',(-0.0765757310810901,-0.134066323362434,
1.11719831593772));
#17556=CARTESIAN_POINT('Ctrl Pts',(-0.0290731934694857,-0.143678417446031,
1.11984570531198));
#17557=CARTESIAN_POINT('Ctrl Pts',(0.01842934414212,-0.153290511529629,
1.12249309468624));
#17558=CARTESIAN_POINT('Ctrl Pts',(0.071170782271703,-0.137012194352758,
1.1251404840605));
#17559=CARTESIAN_POINT('Ctrl Pts',(0.10499283308901,-0.102299771349957,
1.12778787343476));
#17560=CARTESIAN_POINT('Ctrl Pts',(0.138814883906317,-0.0675873483471558,
1.13043526280902));
#17561=CARTESIAN_POINT('Ctrl Pts',(0.153717547411349,-0.0144408195184256,
1.13308265218328));
#17562=CARTESIAN_POINT('Ctrl Pts',(0.142874638214406,0.0327959749574983,
1.13573004155754));
#17563=CARTESIAN_POINT('Ctrl Pts',(0.132031729017462,0.0800327694334235,
1.1383774309318));
#17564=CARTESIAN_POINT('Ctrl Pts',(0.0954432471185425,0.121359829556542,
1.14102482030606));
#17565=CARTESIAN_POINT('Ctrl Pts',(0.0498685966661331,0.137847238945365,
1.14367220968032));
#17566=CARTESIAN_POINT('Ctrl Pts',(0.00429394621372511,0.154334648334189,
1.14631959905458));
#17567=CARTESIAN_POINT('Ctrl Pts',(-0.0502668727921719,0.145982406988718,
1.14896698842884));
#17568=CARTESIAN_POINT('Ctrl Pts',(-0.0888222026239048,0.116616270474356,
1.1516143778031));
#17569=CARTESIAN_POINT('Ctrl Pts',(-0.124357782404925,0.0895501633622979,
1.1540544170073));
#17570=CARTESIAN_POINT('Ctrl Pts',(-0.146296868742479,0.0446329749882746,
1.15649445621151));
#17571=CARTESIAN_POINT('Ctrl Pts',(-0.146552328192774,-6.73160170860698E-5,
1.15893449541571));
#17572=CARTESIAN_POINT('Origin',(0.,0.,0.));
#17573=CARTESIAN_POINT('',(-0.146318311025392,0.000133437649768732,1.21606550458429));
#17574=CARTESIAN_POINT('',(-0.146373054956946,0.000132657382717961,1.20893449541571));
#17575=CARTESIAN_POINT('',(-0.14635,-1.79227059055215E-17,0.));
#17576=CARTESIAN_POINT('Ctrl Pts',(-0.146318311025392,0.000133437649768732,
1.21606550458429));
#17577=CARTESIAN_POINT('Ctrl Pts',(-0.146429658069886,0.0125190846592594,
1.21539220633629));
#17578=CARTESIAN_POINT('Ctrl Pts',(-0.144988168643405,0.0248791929292086,
1.21471890808829));
#17579=CARTESIAN_POINT('Ctrl Pts',(-0.141892968227885,0.0368102906365087,
1.21404560984029));
#17580=CARTESIAN_POINT('Ctrl Pts',(-0.129727599662405,0.083704249513052,
1.21139927996119));
#17581=CARTESIAN_POINT('Ctrl Pts',(-0.0920156607298113,0.123970842060419,
1.20875295008209));
#17582=CARTESIAN_POINT('Ctrl Pts',(-0.0460184991925076,0.139179415364965,
1.20610662020299));
#17583=CARTESIAN_POINT('Ctrl Pts',(-2.13376552038805E-5,0.15438798866951,
1.20346029032389));
#17584=CARTESIAN_POINT('Ctrl Pts',(0.0542610464868107,0.144538542731236,
1.20081396044478));
#17585=CARTESIAN_POINT('Ctrl Pts',(0.091982751999895,0.114139323915075,
1.19816763056568));
#17586=CARTESIAN_POINT('Ctrl Pts',(0.129704457512977,0.0837401050989159,
1.19552130068658));
#17587=CARTESIAN_POINT('Ctrl Pts',(0.150865484397133,0.0327911134048729,
1.19287497080748));
#17588=CARTESIAN_POINT('Ctrl Pts',(0.145780097726084,-0.0153874961003253,
1.19022864092838));
#17589=CARTESIAN_POINT('Ctrl Pts',(0.140694711055036,-0.063566105605525,
1.18758231104927));
#17590=CARTESIAN_POINT('Ctrl Pts',(0.109362910828785,-0.108974332921877,
1.18493598117017));
#17591=CARTESIAN_POINT('Ctrl Pts',(0.0661257549466402,-0.130828118009858,
1.18228965129107));
#17592=CARTESIAN_POINT('Ctrl Pts',(0.0228885990644955,-0.152681903097838,
1.17964332141197));
#17593=CARTESIAN_POINT('Ctrl Pts',(-0.0322539124735426,-0.150981245957443,
1.17699699153287));
#17594=CARTESIAN_POINT('Ctrl Pts',(-0.0740621845924981,-0.126504564117865,
1.17435066165376));
#17595=CARTESIAN_POINT('Ctrl Pts',(-0.115870456711455,-0.102027882278287,
1.17170433177466));
#17596=CARTESIAN_POINT('Ctrl Pts',(-0.144344489411329,-0.0547751757395235,
1.16905800189556));
#17597=CARTESIAN_POINT('Ctrl Pts',(-0.146451269950206,-0.00637475169995868,
1.16641167201646));
#17598=CARTESIAN_POINT('Ctrl Pts',(-0.146543132875163,-0.00426432565444621,
1.1662962828724));
#17599=CARTESIAN_POINT('Ctrl Pts',(-0.146584864748453,-0.00215171749738942,
1.16618089372835));
#17600=CARTESIAN_POINT('Ctrl Pts',(-0.146577386142569,-3.88073511912723E-5,
1.16606550458429));
#17601=CARTESIAN_POINT('Ctrl Pts',(-0.146552328192774,-6.73160170860698E-5,
1.15893449541571));
#17602=CARTESIAN_POINT('Ctrl Pts',(-0.146574036680232,-0.00386586684592084,
1.15914184558577));
#17603=CARTESIAN_POINT('Ctrl Pts',(-0.1464391612665,-0.00766285139452399,
1.15934919575582));
#17604=CARTESIAN_POINT('Ctrl Pts',(-0.146142739258869,-0.0114471821958193,
1.15955654592588));
#17605=CARTESIAN_POINT('Ctrl Pts',(-0.142358105404532,-0.0597644666683822,
1.16220393530014));
#17606=CARTESIAN_POINT('Ctrl Pts',(-0.112238997038288,-0.106019003930254,
1.1648513246744));
#17607=CARTESIAN_POINT('Ctrl Pts',(-0.0695815129186611,-0.129023839960917,
1.16749871404866));
#17608=CARTESIAN_POINT('Ctrl Pts',(-0.026924028799035,-0.15202867599158,
1.17014610342292));
#17609=CARTESIAN_POINT('Ctrl Pts',(0.0282718310739737,-0.151783810791035,
1.17279349279718));
#17610=CARTESIAN_POINT('Ctrl Pts',(0.0707235276354612,-0.128401405199111,
1.17544088217144));
#17611=CARTESIAN_POINT('Ctrl Pts',(0.11317522419695,-0.105018999607187,
1.1780882715457));
#17612=CARTESIAN_POINT('Ctrl Pts',(0.142882757446916,-0.0584990536238821,
1.18073566091996));
#17613=CARTESIAN_POINT('Ctrl Pts',(0.146238551171451,-0.0101500920973681,
1.18338305029422));
#17614=CARTESIAN_POINT('Ctrl Pts',(0.149594344895986,0.0381988694291446,
1.18603043966848));
#17615=CARTESIAN_POINT('Ctrl Pts',(0.12659839909509,0.0883768464988665,
1.18867782904274));
#17616=CARTESIAN_POINT('Ctrl Pts',(0.0877840381772113,0.117399748124142,
1.191325218417));
#17617=CARTESIAN_POINT('Ctrl Pts',(0.0489696772593311,0.146422649749419,
1.19397260779126));
#17618=CARTESIAN_POINT('Ctrl Pts',(-0.00566309877553352,0.154290475930249,
1.19661999716552));
#17619=CARTESIAN_POINT('Ctrl Pts',(-0.0510896721842483,0.137399358129564,
1.19926738653978));
#17620=CARTESIAN_POINT('Ctrl Pts',(-0.0965162455929618,0.12050824032888,
1.20191477591404));
#17621=CARTESIAN_POINT('Ctrl Pts',(-0.132736616375526,0.0788581785466829,
1.2045621652883));
#17622=CARTESIAN_POINT('Ctrl Pts',(-0.143159994183491,0.0315270405159292,
1.20720955466256));
#17623=CARTESIAN_POINT('Ctrl Pts',(-0.145423823013163,0.021247302336111,
1.20778453491361));
#17624=CARTESIAN_POINT('Ctrl Pts',(-0.146470795531708,0.0106995851133921,
1.20835951516466));
#17625=CARTESIAN_POINT('Ctrl Pts',(-0.146373054956946,0.000132657382717961,
1.20893449541571));
#17626=CARTESIAN_POINT('Origin',(0.,0.,0.));
#17627=CARTESIAN_POINT('',(-0.146120596765396,-4.14129048147555E-5,1.26606550458429));
#17628=CARTESIAN_POINT('',(-0.146109918970638,-1.0198006988139E-5,1.25893449541571));
#17629=CARTESIAN_POINT('',(-0.14635,-1.79227059055215E-17,0.));
#17630=CARTESIAN_POINT('Ctrl Pts',(-0.146120596765396,-4.14129048147555E-5,
1.26606550458429));
#17631=CARTESIAN_POINT('Ctrl Pts',(-0.14605219935785,0.0269443530192317,
1.26460351894424));
#17632=CARTESIAN_POINT('Ctrl Pts',(-0.138898723445843,0.053963836666407,
1.26314153330418));
#17633=CARTESIAN_POINT('Ctrl Pts',(-0.124882896249422,0.0767650581554474,
1.26167954766413));
#17634=CARTESIAN_POINT('Ctrl Pts',(-0.0995129464537159,0.118037388097231,
1.25903321778503));
#17635=CARTESIAN_POINT('Ctrl Pts',(-0.051658938874944,0.145488850208621,
1.25638688790592));
#17636=CARTESIAN_POINT('Ctrl Pts',(-0.00322440565727106,0.146554478394238,
1.25374055802682));
#17637=CARTESIAN_POINT('Ctrl Pts',(0.0452101275604033,0.147620106579856,
1.25109422814772));
#17638=CARTESIAN_POINT('Ctrl Pts',(0.0942251864169787,0.122299900839699,
1.24844789826862));
#17639=CARTESIAN_POINT('Ctrl Pts',(0.121385807331354,0.0821833176976391,
1.24580156838952));
#17640=CARTESIAN_POINT('Ctrl Pts',(0.148546428245729,0.0420667345555804,
1.24315523851041));
#17641=CARTESIAN_POINT('Ctrl Pts',(0.153852611217905,-0.0128462259883804,
1.24050890863131));
#17642=CARTESIAN_POINT('Ctrl Pts',(0.134875632820701,-0.0574210379606392,
1.23786257875221));
#17643=CARTESIAN_POINT('Ctrl Pts',(0.115898654423498,-0.101995849932898,
1.23521624887311));
#17644=CARTESIAN_POINT('Ctrl Pts',(0.0726385146569148,-0.136232513333455,
1.23256991899401));
#17645=CARTESIAN_POINT('Ctrl Pts',(0.0248960600935515,-0.144460368686643,
1.2299235891149));
#17646=CARTESIAN_POINT('Ctrl Pts',(-0.0228463944698117,-0.152688224039831,
1.2272772592358));
#17647=CARTESIAN_POINT('Ctrl Pts',(-0.0750711638299551,-0.134907271345651,
1.2246309293567));
#17648=CARTESIAN_POINT('Ctrl Pts',(-0.107874149410843,-0.0992561323957017,
1.2219845994776));
#17649=CARTESIAN_POINT('Ctrl Pts',(-0.132331163880887,-0.072675612185966,
1.2200115678465));
#17650=CARTESIAN_POINT('Ctrl Pts',(-0.145992019903337,-0.0361614337449312,
1.21803853621539));
#17651=CARTESIAN_POINT('Ctrl Pts',(-0.146318311025392,0.000133437649768732,
1.21606550458429));
#17652=CARTESIAN_POINT('Ctrl Pts',(-0.146373054956946,0.000132657382717961,
1.20893449541571));
#17653=CARTESIAN_POINT('Ctrl Pts',(-0.146020767276673,-0.0379538636644633,
1.21100690453892));
#17654=CARTESIAN_POINT('Ctrl Pts',(-0.130797424420382,-0.0762899498869128,
1.21307931366213));
#17655=CARTESIAN_POINT('Ctrl Pts',(-0.104081054125652,-0.103227285106232,
1.21515172278534));
#17656=CARTESIAN_POINT('Ctrl Pts',(-0.0699523514264828,-0.137638258418326,
1.2177991121596));
#17657=CARTESIAN_POINT('Ctrl Pts',(-0.0170685611947798,-0.153447990763203,
1.22044650153386));
#17658=CARTESIAN_POINT('Ctrl Pts',(0.0303468241642401,-0.143414812629152,
1.22309389090812));
#17659=CARTESIAN_POINT('Ctrl Pts',(0.0777622095232573,-0.133381634495101,
1.22574128028238));
#17660=CARTESIAN_POINT('Ctrl Pts',(0.119709190009594,-0.0975055458821257,
1.22838866965664));
#17661=CARTESIAN_POINT('Ctrl Pts',(0.136973893871985,-0.052219638220276,
1.2310360590309));
#17662=CARTESIAN_POINT('Ctrl Pts',(0.154238597734379,-0.00693373055842239,
1.23368344840516));
#17663=CARTESIAN_POINT('Ctrl Pts',(0.146821024972825,0.0477619961523044,
1.23633083777942));
#17664=CARTESIAN_POINT('Ctrl Pts',(0.118118804930222,0.0868140895256425,
1.23897822715368));
#17665=CARTESIAN_POINT('Ctrl Pts',(0.0894165848876198,0.125866182898978,
1.24162561652794));
#17666=CARTESIAN_POINT('Ctrl Pts',(0.0394297175639698,0.149274642934924,
1.2442730059022));
#17667=CARTESIAN_POINT('Ctrl Pts',(-0.00894524413350711,0.146317192515786,
1.24692039527646));
#17668=CARTESIAN_POINT('Ctrl Pts',(-0.0573202058309854,0.143359742096648,
1.24956778465072));
#17669=CARTESIAN_POINT('Ctrl Pts',(-0.104083261902292,0.114036381222425,
1.25221517402498));
#17670=CARTESIAN_POINT('Ctrl Pts',(-0.127814530591109,0.0717787154251623,
1.25486256339924));
#17671=CARTESIAN_POINT('Ctrl Pts',(-0.139981499518435,0.0501133037087236,
1.2562198740714));
#17672=CARTESIAN_POINT('Ctrl Pts',(-0.146094355379323,0.0250479932723348,
1.25757718474355));
#17673=CARTESIAN_POINT('Ctrl Pts',(-0.146109918970638,-1.0198006988139E-5,
1.25893449541571));
#17674=CARTESIAN_POINT('Origin',(0.,0.,0.));
#17675=CARTESIAN_POINT('',(-0.146470135615938,-0.000111966546850736,1.31606550458429));
#17676=CARTESIAN_POINT('',(-0.146410535958061,-0.000127756381200432,1.30893449541571));
#17677=CARTESIAN_POINT('',(-0.14635,-1.79227059055215E-17,0.));
#17678=CARTESIAN_POINT('Ctrl Pts',(-0.146470135615938,-0.000111966546850736,
1.31606550458429));
#17679=CARTESIAN_POINT('Ctrl Pts',(-0.146120207411574,0.0411799307449602,
1.31381483155218));
#17680=CARTESIAN_POINT('Ctrl Pts',(-0.127827491572984,0.0827431563937987,
1.31156415852007));
#17681=CARTESIAN_POINT('Ctrl Pts',(-0.0969137672218927,0.10998333351997,
1.30931348548796));
#17682=CARTESIAN_POINT('Ctrl Pts',(-0.0605655677022408,0.142012194937238,
1.30666715560886));
#17683=CARTESIAN_POINT('Ctrl Pts',(-0.00676890401288169,0.154239532672684,
1.30402082572976));
#17684=CARTESIAN_POINT('Ctrl Pts',(0.0398526445220406,0.14106870189023,
1.30137449585066));
#17685=CARTESIAN_POINT('Ctrl Pts',(0.0864741930569617,0.127897871107775,
1.29872816597155));
#17686=CARTESIAN_POINT('Ctrl Pts',(0.125920626437448,0.0893288718074177,
1.29608183609245));
#17687=CARTESIAN_POINT('Ctrl Pts',(0.14013669149516,0.0430153417578024,
1.29343550621335));
#17688=CARTESIAN_POINT('Ctrl Pts',(0.154352756552873,-0.00329818829181684,
1.29078917633425));
#17689=CARTESIAN_POINT('Ctrl Pts',(0.143338453287813,-0.0573562490906975,
1.28814284645515));
#17690=CARTESIAN_POINT('Ctrl Pts',(0.112135201594409,-0.0944156157243562,
1.28549651657604));
#17691=CARTESIAN_POINT('Ctrl Pts',(0.0809319499010078,-0.131474982358013,
1.28285018669694));
#17692=CARTESIAN_POINT('Ctrl Pts',(0.0295397497792676,-0.151535654826449,
1.28020385681784));
#17693=CARTESIAN_POINT('Ctrl Pts',(-0.0185183802362589,-0.1454155477333,
1.27755752693874));
#17694=CARTESIAN_POINT('Ctrl Pts',(-0.066576510251784,-0.139295440640151,
1.27491119705964));
#17695=CARTESIAN_POINT('Ctrl Pts',(-0.111300570161094,-0.106994553985419,
1.27226486718053));
#17696=CARTESIAN_POINT('Ctrl Pts',(-0.13221965410943,-0.0632975117719662,
1.26961853730143));
#17697=CARTESIAN_POINT('Ctrl Pts',(-0.141581826511298,-0.0437412423069929,
1.26843419306239));
#17698=CARTESIAN_POINT('Ctrl Pts',(-0.146176005022067,-0.0219023912433209,
1.26724984882334));
#17699=CARTESIAN_POINT('Ctrl Pts',(-0.146120596765396,-4.14129048147555E-5,
1.26606550458429));
#17700=CARTESIAN_POINT('Ctrl Pts',(-0.146109918970638,-1.0198006988139E-5,
1.25893449541571));
#17701=CARTESIAN_POINT('Ctrl Pts',(-0.146124711647138,-0.0238271763493914,
1.26022457411781));
#17702=CARTESIAN_POINT('Ctrl Pts',(-0.140631289159497,-0.0476377233371588,
1.26151465281992));
#17703=CARTESIAN_POINT('Ctrl Pts',(-0.129592576141605,-0.0685164391025303,
1.26280473152202));
#17704=CARTESIAN_POINT('Ctrl Pts',(-0.106939871696956,-0.111361957112663,
1.26545212089628));
#17705=CARTESIAN_POINT('Ctrl Pts',(-0.0609349815013302,-0.141861022412626,
1.26809951027054));
#17706=CARTESIAN_POINT('Ctrl Pts',(-0.0126505083952331,-0.146043496451057,
1.2707468996448));
#17707=CARTESIAN_POINT('Ctrl Pts',(0.0356339647108625,-0.150225970489488,
1.27339428901906));
#17708=CARTESIAN_POINT('Ctrl Pts',(0.0861980207274291,-0.128091853266388,
1.27604167839332));
#17709=CARTESIAN_POINT('Ctrl Pts',(0.11588072467734,-0.0897797074320025,
1.27868906776758));
#17710=CARTESIAN_POINT('Ctrl Pts',(0.145563428627253,-0.0514675615976161,
1.28133645714184));
#17711=CARTESIAN_POINT('Ctrl Pts',(0.154364780510509,0.00302261284805656,
1.2839838465161));
#17712=CARTESIAN_POINT('Ctrl Pts',(0.138253309066183,0.0487315170146188,
1.28663123589036));
#17713=CARTESIAN_POINT('Ctrl Pts',(0.122141837621857,0.0944404211811797,
1.28927862526462));
#17714=CARTESIAN_POINT('Ctrl Pts',(0.0811175428499519,0.131368055068631,
1.29192601463888));
#17715=CARTESIAN_POINT('Ctrl Pts',(0.0339716590485425,0.142599665496764,
1.29457340401314));
#17716=CARTESIAN_POINT('Ctrl Pts',(-0.013174224752867,0.153831275924897,
1.2972207933874));
#17717=CARTESIAN_POINT('Ctrl Pts',(-0.0664416975837803,0.139366862893713,
1.29986818276166));
#17718=CARTESIAN_POINT('Ctrl Pts',(-0.101431520699135,0.105831870563862,
1.30251557213592));
#17719=CARTESIAN_POINT('Ctrl Pts',(-0.129710573305276,0.0787286237393239,
1.30465521322918));
#17720=CARTESIAN_POINT('Ctrl Pts',(-0.146050663974784,0.0391684733249047,
1.30679485432245));
#17721=CARTESIAN_POINT('Ctrl Pts',(-0.146410535958061,-0.000127756381200432,
1.30893449541571));
#17722=CARTESIAN_POINT('Origin',(0.,0.,0.));
#17723=CARTESIAN_POINT('',(-0.146471469669193,0.000111495080380188,1.36606550458429));
#17724=CARTESIAN_POINT('',(-0.146526884620975,8.5711493927648E-5,1.35893449541571));
#17725=CARTESIAN_POINT('',(-0.14635,-1.79227059055215E-17,0.));
#17726=CARTESIAN_POINT('Ctrl Pts',(-0.146471469669193,0.000111495080380188,
1.36606550458429));
#17727=CARTESIAN_POINT('Ctrl Pts',(-0.146532402405025,0.0073220458586883,
1.36567247403923));
#17728=CARTESIAN_POINT('Ctrl Pts',(-0.146045973070864,0.0145243451116175,
1.36527944349416));
#17729=CARTESIAN_POINT('Ctrl Pts',(-0.144983764805735,0.0216407019395156,
1.3648864129491));
#17730=CARTESIAN_POINT('Ctrl Pts',(-0.137831767320671,0.0695561322809842,
1.36224008307));
#17731=CARTESIAN_POINT('Ctrl Pts',(-0.104576727819841,0.113575347233418,
1.3595937531909));
#17732=CARTESIAN_POINT('Ctrl Pts',(-0.060440002550743,0.133550058215342,
1.3569474233118));
#17733=CARTESIAN_POINT('Ctrl Pts',(-0.0163032772816473,0.153524769197265,
1.35430109343269));
#17734=CARTESIAN_POINT('Ctrl Pts',(0.0387151337557165,0.149454976208681,
1.35165476355359));
#17735=CARTESIAN_POINT('Ctrl Pts',(0.0794324390145508,0.123203488242689,
1.34900843367449));
#17736=CARTESIAN_POINT('Ctrl Pts',(0.120149744273387,0.0969520002766962,
1.34636210379539));
#17737=CARTESIAN_POINT('Ctrl Pts',(0.146565943753694,0.048518817333291,
1.34371577391629));
#17738=CARTESIAN_POINT('Ctrl Pts',(0.14658992694451,7.25688577880009E-5,
1.34106944403718));
#17739=CARTESIAN_POINT('Ctrl Pts',(0.146613910135327,-0.0483736796177136,
1.33842311415808));
#17740=CARTESIAN_POINT('Ctrl Pts',(0.120245677036657,-0.0968329936253116,
1.33577678427898));
#17741=CARTESIAN_POINT('Ctrl Pts',(0.0795543829983497,-0.123124782547022,
1.33313045439988));
#17742=CARTESIAN_POINT('Ctrl Pts',(0.0388630889600415,-0.149416571468734,
1.33048412452078));
#17743=CARTESIAN_POINT('Ctrl Pts',(-0.0161512660179049,-0.153540835304554,
1.32783779464168));
#17744=CARTESIAN_POINT('Ctrl Pts',(-0.0603077462478081,-0.133609833714981,
1.32519146476257));
#17745=CARTESIAN_POINT('Ctrl Pts',(-0.10446422647771,-0.113678832125408,
1.32254513488347));
#17746=CARTESIAN_POINT('Ctrl Pts',(-0.137762831959571,-0.0696925651104417,
1.31989880500437));
#17747=CARTESIAN_POINT('Ctrl Pts',(-0.144962267025529,-0.0217842390534145,
1.31725247512527));
#17748=CARTESIAN_POINT('Ctrl Pts',(-0.146038665626028,-0.0146213916011371,
1.31685681827827));
#17749=CARTESIAN_POINT('Ctrl Pts',(-0.146531651210624,-0.00737087161912708,
1.31646116143128));
#17750=CARTESIAN_POINT('Ctrl Pts',(-0.146470135615938,-0.000111966546850736,
1.31606550458429));
#17751=CARTESIAN_POINT('Ctrl Pts',(-0.146410535958061,-0.000127756381200432,
1.30893449541571));
#17752=CARTESIAN_POINT('Ctrl Pts',(-0.146495935505426,-0.00945296197092968,
1.30944224369671));
#17753=CARTESIAN_POINT('Ctrl Pts',(-0.145681427739287,-0.018763305174839,
1.3099499919777));
#17754=CARTESIAN_POINT('Ctrl Pts',(-0.143913007029536,-0.0278887903271487,
1.3104577402587));
#17755=CARTESIAN_POINT('Ctrl Pts',(-0.134692496844786,-0.0754688872597875,
1.31310512963296));
#17756=CARTESIAN_POINT('Ctrl Pts',(-0.0995393030754929,-0.118023509496548,
1.31575251900722));
#17757=CARTESIAN_POINT('Ctrl Pts',(-0.0545553941775042,-0.136060454153345,
1.31839990838148));
#17758=CARTESIAN_POINT('Ctrl Pts',(-0.00957148527951295,-0.154097398810142,
1.32104729775574));
#17759=CARTESIAN_POINT('Ctrl Pts',(0.0452431387471776,-0.14761666588697,
1.32369468713));
#17760=CARTESIAN_POINT('Ctrl Pts',(0.0847805644327026,-0.119586763955155,
1.32634207650426));
#17761=CARTESIAN_POINT('Ctrl Pts',(0.124317990118227,-0.09155686202334,
1.32898946587852));
#17762=CARTESIAN_POINT('Ctrl Pts',(0.148578217462589,-0.041977791082884,
1.33163685525278));
#17763=CARTESIAN_POINT('Ctrl Pts',(0.146448816178573,0.00644068764408242,
1.33428424462704));
#17764=CARTESIAN_POINT('Ctrl Pts',(0.144319414894557,0.0548591663710502,
1.3369316340013));
#17765=CARTESIAN_POINT('Ctrl Pts',(0.115800384982161,0.102117052884526,
1.33957902337556));
#17766=CARTESIAN_POINT('Ctrl Pts',(0.0739549070570988,0.126567807678519,
1.34222641274982));
#17767=CARTESIAN_POINT('Ctrl Pts',(0.0321094291320376,0.151018562472512,
1.34487380212408));
#17768=CARTESIAN_POINT('Ctrl Pts',(-0.0230624968056921,0.152662185547021,
1.34752119149834));
#17769=CARTESIAN_POINT('Ctrl Pts',(-0.0662892946253695,0.1307458130856,
1.3501685808726));
#17770=CARTESIAN_POINT('Ctrl Pts',(-0.109516092445046,0.10882944062418,
1.35281597024686));
#17771=CARTESIAN_POINT('Ctrl Pts',(-0.140797762146673,0.0633530726268328,
1.35546335962112));
#17772=CARTESIAN_POINT('Ctrl Pts',(-0.145805692234247,0.0151472216574969,
1.35811074899538));
#17773=CARTESIAN_POINT('Ctrl Pts',(-0.146325105122407,0.0101474034011793,
1.35838533113549));
#17774=CARTESIAN_POINT('Ctrl Pts',(-0.146561879835735,0.00511822289583405,
1.3586599132756));
#17775=CARTESIAN_POINT('Ctrl Pts',(-0.146526884620975,8.5711493927648E-5,
1.35893449541571));
#17776=CARTESIAN_POINT('Origin',(0.,0.,0.));
#17777=CARTESIAN_POINT('',(-0.146120987371435,4.2191387702159E-5,1.41606550458429));
#17778=CARTESIAN_POINT('',(-0.146148882937928,7.6306569664006E-5,1.40893449541571));
#17779=CARTESIAN_POINT('',(-0.14635,-1.79227059055215E-17,0.));
#17780=CARTESIAN_POINT('Ctrl Pts',(-0.146120987371435,4.2191387702159E-5,
1.41606550458429));
#17781=CARTESIAN_POINT('Ctrl Pts',(-0.146177309023295,0.021854523983563,
1.41488378664717));
#17782=CARTESIAN_POINT('Ctrl Pts',(-0.141604359564088,0.0436444172696427,
1.41370206871005));
#17783=CARTESIAN_POINT('Ctrl Pts',(-0.132282279973341,0.0631665524487371,
1.41252035077294));
#17784=CARTESIAN_POINT('Ctrl Pts',(-0.1114064880593,0.106884268839086,1.40987402089383));
#17785=CARTESIAN_POINT('Ctrl Pts',(-0.0667143915920224,0.139229456738304,
1.40722769101473));
#17786=CARTESIAN_POINT('Ctrl Pts',(-0.0186623352932378,0.145397151366753,
1.40458136113563));
#17787=CARTESIAN_POINT('Ctrl Pts',(0.0293897210055454,0.151564845995202,
1.40193503125653));
#17788=CARTESIAN_POINT('Ctrl Pts',(0.0808017371358351,0.131555047352884,
1.39928870137743));
#17789=CARTESIAN_POINT('Ctrl Pts',(0.112041660826149,0.0945265884816804,
1.39664237149832));
#17790=CARTESIAN_POINT('Ctrl Pts',(0.143281584516463,0.0574981296104763,
1.39399604161922));
#17791=CARTESIAN_POINT('Ctrl Pts',(0.154349415766802,0.00345101051038574,
1.39134971174012));
#17792=CARTESIAN_POINT('Ctrl Pts',(0.140179214932283,-0.0428765696854336,
1.38870338186102));
#17793=CARTESIAN_POINT('Ctrl Pts',(0.126009014097764,-0.089204149881253,
1.38605705198192));
#17794=CARTESIAN_POINT('Ctrl Pts',(0.0866007811783877,-0.127812191172801,
1.38341072210282));
#17795=CARTESIAN_POINT('Ctrl Pts',(0.0399922944706322,-0.14102917638501,
1.38076439222371));
#17796=CARTESIAN_POINT('Ctrl Pts',(-0.00661619223712474,-0.15424616159722,
1.37811806234461));
#17797=CARTESIAN_POINT('Ctrl Pts',(-0.060424932733261,-0.142072090730089,
1.37547173246551));
#17798=CARTESIAN_POINT('Ctrl Pts',(-0.0968048252466797,-0.110079232431271,
1.37282540258641));
#17799=CARTESIAN_POINT('Ctrl Pts',(-0.127781608685608,-0.08283792481198,
1.37057210325237));
#17800=CARTESIAN_POINT('Ctrl Pts',(-0.146122133733866,-0.0412276055847571,
1.36831880391833));
#17801=CARTESIAN_POINT('Ctrl Pts',(-0.146471469669193,0.000111495080380188,
1.36606550458429));
#17802=CARTESIAN_POINT('Ctrl Pts',(-0.146526884620975,8.5711493927648E-5,
1.35893449541571));
#17803=CARTESIAN_POINT('Ctrl Pts',(-0.146224472749943,-0.0434028397118431,
1.36130730264986));
#17804=CARTESIAN_POINT('Ctrl Pts',(-0.125627402569456,-0.0871401285467012,
1.36368010988401));
#17805=CARTESIAN_POINT('Ctrl Pts',(-0.0917490966422633,-0.114327780902106,
1.36605291711816));
#17806=CARTESIAN_POINT('Ctrl Pts',(-0.0539503804891888,-0.144661598551044,
1.36870030649242));
#17807=CARTESIAN_POINT('Ctrl Pts',(0.00038124229047478,-0.154393899907594,
1.37134769586668));
#17808=CARTESIAN_POINT('Ctrl Pts',(0.0463590973565905,-0.139066790892088,
1.37399508524094));
#17809=CARTESIAN_POINT('Ctrl Pts',(0.0923369524227062,-0.123739681876581,
1.3766424746152));
#17810=CARTESIAN_POINT('Ctrl Pts',(0.129961039775272,-0.083353162489017,
1.37928986398946));
#17811=CARTESIAN_POINT('Ctrl Pts',(0.141997595260484,-0.0364063334065561,
1.38193725336372));
#17812=CARTESIAN_POINT('Ctrl Pts',(0.154034150745695,0.0105404956759021,
1.38458464273798));
#17813=CARTESIAN_POINT('Ctrl Pts',(0.140483174363557,0.0640476344532581,
1.38723203211224));
#17814=CARTESIAN_POINT('Ctrl Pts',(0.10755170844225,0.0996060653705087,
1.3898794214865));
#17815=CARTESIAN_POINT('Ctrl Pts',(0.0746202425209409,0.135164496287762,
1.39252681086076));
#17816=CARTESIAN_POINT('Ctrl Pts',(0.0223082870604623,0.152774219344908,
1.39517420023502));
#17817=CARTESIAN_POINT('Ctrl Pts',(-0.025422593472234,0.144369075867769,
1.39782158960928));
#17818=CARTESIAN_POINT('Ctrl Pts',(-0.073153474004929,0.135963932390631,
1.40046897898354));
#17819=CARTESIAN_POINT('Ctrl Pts',(-0.11630327960984,0.101543922379208,
1.4031163683578));
#17820=CARTESIAN_POINT('Ctrl Pts',(-0.135107186188192,0.0568751802851974,
1.40576375773206));
#17821=CARTESIAN_POINT('Ctrl Pts',(-0.142614236437708,0.0390421576584788,
1.40682067029328));
#17822=CARTESIAN_POINT('Ctrl Pts',(-0.14624095998336,0.0195756595648056,
1.40787758285449));
#17823=CARTESIAN_POINT('Ctrl Pts',(-0.146148882937928,7.6306569664006E-5,
1.40893449541571));
#17824=CARTESIAN_POINT('Origin',(0.,0.,0.));
#17825=CARTESIAN_POINT('',(-0.14631473222987,-0.000131398079681141,1.46606550458429));
#17826=CARTESIAN_POINT('',(-0.146248097568756,-0.000123763188177425,1.45893449541571));
#17827=CARTESIAN_POINT('',(-0.14635,-1.79227059055215E-17,0.));
#17828=CARTESIAN_POINT('Ctrl Pts',(-0.14631473222987,-0.000131398079681141,
1.46606550458429));
#17829=CARTESIAN_POINT('Ctrl Pts',(-0.145989697979493,0.0361157155227289,
1.46409509925512));
#17830=CARTESIAN_POINT('Ctrl Pts',(-0.132370868650209,0.0725796635271419,
1.46212469392594));
#17831=CARTESIAN_POINT('Ctrl Pts',(-0.107973319296019,0.0991484059484618,
1.46015428859677));
#17832=CARTESIAN_POINT('Ctrl Pts',(-0.0752064754000165,0.134831245351468,
1.45750795871767));
#17833=CARTESIAN_POINT('Ctrl Pts',(-0.0229974942306327,0.152665588379184,
1.45486162883857));
#17834=CARTESIAN_POINT('Ctrl Pts',(0.0247535192036911,0.144485406820094,
1.45221529895946));
#17835=CARTESIAN_POINT('Ctrl Pts',(0.0725045326380122,0.136305225261004,
1.44956896908036));
#17836=CARTESIAN_POINT('Ctrl Pts',(0.115797578337275,0.102110519115111,
1.44692263920126));
#17837=CARTESIAN_POINT('Ctrl Pts',(0.134818450998255,0.0575543070937695,
1.44427630932216));
#17838=CARTESIAN_POINT('Ctrl Pts',(0.153839323659235,0.0129980950724284,
1.44162997944306));
#17839=CARTESIAN_POINT('Ctrl Pts',(0.148588023281934,-0.0419196228243577,
1.43898364956396));
#17840=CARTESIAN_POINT('Ctrl Pts',(0.121467255745355,-0.082062966762292,
1.43633731968485));
#17841=CARTESIAN_POINT('Ctrl Pts',(0.0943464882087764,-0.122206310700226,
1.43369098980575));
#17842=CARTESIAN_POINT('Ctrl Pts',(0.0453562535129183,-0.147575280679306,
1.43104465992665));
#17843=CARTESIAN_POINT('Ctrl Pts',(-0.00307937473935208,-0.146557666176543,
1.42839833004755));
#17844=CARTESIAN_POINT('Ctrl Pts',(-0.0515150029916225,-0.14554005167378,
1.42575200016845));
#17845=CARTESIAN_POINT('Ctrl Pts',(-0.0993960248003067,-0.118135852689175,
1.42310567028934));
#17846=CARTESIAN_POINT('Ctrl Pts',(-0.124806792024246,-0.0768886307561326,
1.42045934041024));
#17847=CARTESIAN_POINT('Ctrl Pts',(-0.138870387581649,-0.0540603453281256,
1.41899472846826));
#17848=CARTESIAN_POINT('Ctrl Pts',(-0.146051182757901,-0.0269918425378075,
1.41753011652627));
#17849=CARTESIAN_POINT('Ctrl Pts',(-0.146120987371435,4.2191387702159E-5,
1.41606550458429));
#17850=CARTESIAN_POINT('Ctrl Pts',(-0.146148882937928,7.6306569664006E-5,
1.40893449541571));
#17851=CARTESIAN_POINT('Ctrl Pts',(-0.146010322369016,-0.0292669616874671,
1.41052497222875));
#17852=CARTESIAN_POINT('Ctrl Pts',(-0.137450455640384,-0.0586846305953837,
1.4121154490418));
#17853=CARTESIAN_POINT('Ctrl Pts',(-0.121019719714466,-0.0827222215753489,
1.41370592585484));
#17854=CARTESIAN_POINT('Ctrl Pts',(-0.0936703391105966,-0.122733407165291,
1.4163533152291));
#17855=CARTESIAN_POINT('Ctrl Pts',(-0.0445135703510636,-0.147838304168576,
1.41900070460336));
#17856=CARTESIAN_POINT('Ctrl Pts',(0.00393424939099551,-0.146537573651384,
1.42164809397762));
#17857=CARTESIAN_POINT('Ctrl Pts',(0.0523820691330518,-0.145236843134192,
1.42429548335188));
#17858=CARTESIAN_POINT('Ctrl Pts',(0.100120939857634,-0.117530485096527,
1.42694287272614));
#17859=CARTESIAN_POINT('Ctrl Pts',(0.125284029446909,-0.0761094471358441,
1.4295902621004));
#17860=CARTESIAN_POINT('Ctrl Pts',(0.150447119036187,-0.0346884091751576,
1.43223765147466));
#17861=CARTESIAN_POINT('Ctrl Pts',(0.153034427490153,0.020447308708549,
1.43488504084892));
#17862=CARTESIAN_POINT('Ctrl Pts',(0.13186079120536,0.0640427391611241,
1.43753243022318));
#17863=CARTESIAN_POINT('Ctrl Pts',(0.110687154920568,0.107638169613697,
1.44017981959744));
#17864=CARTESIAN_POINT('Ctrl Pts',(0.0657525738970213,0.139693312635139,
1.4428272089717));
#17865=CARTESIAN_POINT('Ctrl Pts',(0.0176394768514684,0.145525221357757,
1.44547459834596));
#17866=CARTESIAN_POINT('Ctrl Pts',(-0.0304736201940859,0.151357130080375,
1.44812198772022));
#17867=CARTESIAN_POINT('Ctrl Pts',(-0.0817652332616461,0.130965804504167,
1.45076937709448));
#17868=CARTESIAN_POINT('Ctrl Pts',(-0.112741325423428,0.0936916042199666,
1.45341676646874));
#17869=CARTESIAN_POINT('Ctrl Pts',(-0.134261605244105,0.0677957870194472,
1.45525600945106));
#17870=CARTESIAN_POINT('Ctrl Pts',(-0.145976367207401,0.0337512577971725,
1.45709525243339));
#17871=CARTESIAN_POINT('Ctrl Pts',(-0.146248097568756,-0.000123763188177425,
1.45893449541571));
#17872=CARTESIAN_POINT('Origin',(0.,0.,-0.0924367114736175));
#17873=CARTESIAN_POINT('',(-0.117746618301147,-0.000105742458702955,1.48256328852638));
#17874=CARTESIAN_POINT('',(-0.117971241274414,-5.28325160115065E-6,1.49243671147361));
#17875=CARTESIAN_POINT('',(-0.117775,2.85464118895969E-14,-0.0924367114736175));
#17876=CARTESIAN_POINT('',(-0.117668597464313,0.00500517689812599,1.532225));
#17877=CARTESIAN_POINT('Ctrl Pts',(-0.117746618301147,-0.000105742458702949,
1.48256328852638));
#17878=CARTESIAN_POINT('Ctrl Pts',(-0.117836347163251,-0.0101121102621826,
1.48323921307631));
#17879=CARTESIAN_POINT('Ctrl Pts',(-0.112089674709738,-0.0591937430214443,
1.48656146750534));
#17880=CARTESIAN_POINT('Ctrl Pts',(-0.0435804807853106,-0.132222740314769,
1.49253005181348));
#17881=CARTESIAN_POINT('Ctrl Pts',(0.0874774386997331,-0.108286040948335,
1.50046904145078));
#17882=CARTESIAN_POINT('Ctrl Pts',(0.138385550162814,0.0147146982980264,
1.50840803108809));
#17883=CARTESIAN_POINT('Ctrl Pts',(0.0627460642121078,0.124368470664037,
1.51634702072539));
#17884=CARTESIAN_POINT('Ctrl Pts',(-0.0706026869052757,0.119928391791904,
1.5242860103627));
#17885=CARTESIAN_POINT('Ctrl Pts',(-0.116004137797729,0.0441355889673283,
1.5295786701209));
#17886=CARTESIAN_POINT('Ctrl Pts',(-0.117668597464313,0.00500517689812487,
1.532225));
#17887=CARTESIAN_POINT('',(-0.0334019664627544,0.1129391839063,1.53222500000001));
#17888=CARTESIAN_POINT('Origin',(0.,0.,1.532225));
#17889=CARTESIAN_POINT('Ctrl Pts',(-0.117971276761593,-5.28420699491729E-6,
1.49243671147361));
#17890=CARTESIAN_POINT('Ctrl Pts',(-0.117971582784674,-0.000385634193345565,
1.49246252744444));
#17891=CARTESIAN_POINT('Ctrl Pts',(-0.117794795258817,-0.0397700451254522,
1.49513573278954));
#17892=CARTESIAN_POINT('Ctrl Pts',(-0.0742871760264013,-0.117748889605885,
1.50045632750888));
#17893=CARTESIAN_POINT('Ctrl Pts',(0.0586284551779338,-0.126233948370975,
1.50839849563167));
#17894=CARTESIAN_POINT('Ctrl Pts',(0.137995068118234,-0.019163470063063,
1.51634066375444));
#17895=CARTESIAN_POINT('Ctrl Pts',(0.0906261803825392,0.105639137646141,
1.52428283187723));
#17896=CARTESIAN_POINT('Ctrl Pts',(0.00417072711528833,0.124051375507138,
1.52957761062575));
#17897=CARTESIAN_POINT('Ctrl Pts',(-0.0334019664627544,0.1129391839063,
1.53222500000001));
#17898=CARTESIAN_POINT('Origin',(0.,0.,-0.0924367114736175));
#17899=CARTESIAN_POINT('',(-0.117590702341447,3.3953472435133E-5,1.43256328852638));
#17900=CARTESIAN_POINT('',(-0.117692994131604,-9.95982882293356E-5,1.44243671147361));
#17901=CARTESIAN_POINT('',(-0.117775,2.85464118895969E-14,-0.0924367114736175));
#17902=CARTESIAN_POINT('Ctrl Pts',(-0.117590702341447,3.39534724351446E-5,
1.43256328852638));
#17903=CARTESIAN_POINT('Ctrl Pts',(-0.117534527156218,-0.0217216553118358,
1.43402790046837));
#17904=CARTESIAN_POINT('Ctrl Pts',(-0.101314495966545,-0.0828641818343832,
1.43813884228945));
#17905=CARTESIAN_POINT('Ctrl Pts',(-0.00292444232197888,-0.139176693688359,
1.44489611398964));
#17906=CARTESIAN_POINT('Ctrl Pts',(0.115350068603298,-0.0779297424218237,
1.45283510362695));
#17907=CARTESIAN_POINT('Ctrl Pts',(0.128028003046829,0.0546551750765237,
1.46077409326425));
#17908=CARTESIAN_POINT('Ctrl Pts',(0.0235079116789307,0.137209630484779,
1.46871308290156));
#17909=CARTESIAN_POINT('Ctrl Pts',(-0.0918059616614023,0.0978189523496558,
1.47597614798894));
#17910=CARTESIAN_POINT('Ctrl Pts',(-0.117485047349053,0.0290640819657798,
1.48059288319721));
#17911=CARTESIAN_POINT('Ctrl Pts',(-0.117746618301147,-0.000105742458702949,
1.48256328852638));
#17912=CARTESIAN_POINT('Ctrl Pts',(-0.117692994131604,-9.9598288229346E-5,
1.44243671147361));
#17913=CARTESIAN_POINT('Ctrl Pts',(-0.117789077779518,-0.0120777797952868,
1.44324485786555));
#17914=CARTESIAN_POINT('Ctrl Pts',(-0.110597905189529,-0.0631824179582176,
1.44670039363175));
#17915=CARTESIAN_POINT('Ctrl Pts',(-0.0368790902657646,-0.134252921254984,
1.45280331877221));
#17916=CARTESIAN_POINT('Ctrl Pts',(0.0928396680879532,-0.103751556080299,
1.46074548689499));
#17917=CARTESIAN_POINT('Ctrl Pts',(0.137511141307062,0.0217950526079239,
1.46868765501776));
#17918=CARTESIAN_POINT('Ctrl Pts',(0.0562018483347667,0.127378648737854,
1.47662982314055));
#17919=CARTESIAN_POINT('Ctrl Pts',(-0.0761502833827582,0.1162998103107,
1.48454617529249));
#17920=CARTESIAN_POINT('Ctrl Pts',(-0.117940200573233,0.0386186906477724,
1.48981513807018));
#17921=CARTESIAN_POINT('Ctrl Pts',(-0.117971276761593,-5.28420699491729E-6,
1.49243671147361));
#17922=CARTESIAN_POINT('Origin',(0.,0.,-0.0924367114736175));
#17923=CARTESIAN_POINT('',(-0.117872752581409,8.97255421561373E-5,1.38256328852638));
#17924=CARTESIAN_POINT('',(-0.117613151267609,6.14076272390171E-5,1.39243671147361));
#17925=CARTESIAN_POINT('',(-0.117775,2.85464118895969E-14,-0.0924367114736175));
#17926=CARTESIAN_POINT('Ctrl Pts',(-0.117872752581409,8.97255421561322E-5,
1.38256328852638));
#17927=CARTESIAN_POINT('Ctrl Pts',(-0.117591624875346,-0.0331778698171688,
1.38481658786042));
#17928=CARTESIAN_POINT('Ctrl Pts',(-0.0854981695600773,-0.105990339321694,
1.38971621707357));
#17929=CARTESIAN_POINT('Ctrl Pts',(0.0379781508110965,-0.133926497290667,
1.39726217616581));
#17930=CARTESIAN_POINT('Ctrl Pts',(0.133119345865688,-0.0407171622080862,
1.40520116580311));
#17931=CARTESIAN_POINT('Ctrl Pts',(0.106398871137127,0.0897659150453452,
1.41314015544042));
#17932=CARTESIAN_POINT('Ctrl Pts',(-0.0177224175491345,0.138074504763813,
1.42107914507772));
#17933=CARTESIAN_POINT('Ctrl Pts',(-0.105714817800915,0.0743914165933911,
1.42755352277305));
#17934=CARTESIAN_POINT('Ctrl Pts',(-0.11763602712824,0.0175874039095825,
1.43138157058926));
#17935=CARTESIAN_POINT('Ctrl Pts',(-0.117590702341447,3.39534724351446E-5,
1.43256328852638));
#17936=CARTESIAN_POINT('Ctrl Pts',(-0.117613151267609,6.1407627239024E-5,
1.39243671147361));
#17937=CARTESIAN_POINT('Ctrl Pts',(-0.117501644803633,-0.0235525549213426,
1.39402718828666));
#17938=CARTESIAN_POINT('Ctrl Pts',(-0.0991469449676741,-0.0866320980727062,
1.39826505447396));
#17939=CARTESIAN_POINT('Ctrl Pts',(0.00373660876362508,-0.139175849115243,
1.40515031003553));
#17940=CARTESIAN_POINT('Ctrl Pts',(0.118990018389619,-0.0722858665142316,
1.41309247815831));
#17941=CARTESIAN_POINT('Ctrl Pts',(0.125236419206141,0.0608253567263532,
1.42103464628109));
#17942=CARTESIAN_POINT('Ctrl Pts',(0.0167532566496359,0.13821437898841,
1.42897681440387));
#17943=CARTESIAN_POINT('Ctrl Pts',(-0.0944771051913143,0.0939940009069027,
1.43611083613471));
#17944=CARTESIAN_POINT('Ctrl Pts',(-0.117474319425011,0.0271612872365273,
1.44059746849129));
#17945=CARTESIAN_POINT('Ctrl Pts',(-0.117692994131604,-9.9598288229346E-5,
1.44243671147361));
#17946=CARTESIAN_POINT('Origin',(0.,0.,-0.0924367114736175));
#17947=CARTESIAN_POINT('',(-0.117871679003533,-9.01049542302267E-5,1.33256328852638));
#17948=CARTESIAN_POINT('',(-0.117917347702326,6.89762296073142E-5,1.34243671147361));
#17949=CARTESIAN_POINT('',(-0.117775,2.85464118895969E-14,-0.0924367114736175));
#17950=CARTESIAN_POINT('Ctrl Pts',(-0.117871679003533,-9.01049542302501E-5,
1.33256328852638));
#17951=CARTESIAN_POINT('Ctrl Pts',(-0.117921183610054,-0.00593170075121234,
1.33295894537338));
#17952=CARTESIAN_POINT('Ctrl Pts',(-0.114870949065289,-0.0507926200311143,
1.33600093209947));
#17953=CARTESIAN_POINT('Ctrl Pts',(-0.0572704544775333,-0.126880813469472,
1.34168924870467));
#17954=CARTESIAN_POINT('Ctrl Pts',(0.0755477687720905,-0.116923823242002,
1.34962823834197));
#17955=CARTESIAN_POINT('Ctrl Pts',(0.13920718769651,6.89141801743488E-5,
1.35756722797928));
#17956=CARTESIAN_POINT('Ctrl Pts',(0.0754319660950179,0.116998564767658,
1.36550621761658));
#17957=CARTESIAN_POINT('Ctrl Pts',(-0.0573960494825499,0.126824048933643,
1.37344520725389));
#17958=CARTESIAN_POINT('Ctrl Pts',(-0.11489462347839,0.0507140179075799,
1.37913089755716));
#17959=CARTESIAN_POINT('Ctrl Pts',(-0.117921788132912,0.00589240827474643,
1.38217025798132));
#17960=CARTESIAN_POINT('Ctrl Pts',(-0.117872752581409,8.97255421561322E-5,
1.38256328852638));
#17961=CARTESIAN_POINT('Ctrl Pts',(-0.117917347702326,6.89762296073276E-5,
1.34243671147361));
#17962=CARTESIAN_POINT('Ctrl Pts',(-0.117673982084908,-0.0349283870656527,
1.34480951870776));
#17963=CARTESIAN_POINT('Ctrl Pts',(-0.0826049238592893,-0.109396528181867,
1.34982971531618));
#17964=CARTESIAN_POINT('Ctrl Pts',(0.0440301174146577,-0.132080378229483,
1.35749730129884));
#17965=CARTESIAN_POINT('Ctrl Pts',(0.13486394497766,-0.0345773583278084,
1.36543946942163));
#17966=CARTESIAN_POINT('Ctrl Pts',(0.102148545386143,0.0946020732301706,
1.3733816375444));
#17967=CARTESIAN_POINT('Ctrl Pts',(-0.0241454188302812,0.137116288461919,
1.38132380566719));
#17968=CARTESIAN_POINT('Ctrl Pts',(-0.107458038693719,0.07065895059964,
1.38767549697692));
#17969=CARTESIAN_POINT('Ctrl Pts',(-0.117687250167678,0.015753490298928,
1.3913797989124));
#17970=CARTESIAN_POINT('Ctrl Pts',(-0.117613151267609,6.1407627239024E-5,
1.39243671147361));
#17971=CARTESIAN_POINT('Origin',(0.,0.,-0.0924367114736175));
#17972=CARTESIAN_POINT('',(-0.117590388001671,-3.33269891443968E-5,1.28256328852638));
#17973=CARTESIAN_POINT('',(-0.117823716245033,-0.000102811805890834,1.29243671147362));
#17974=CARTESIAN_POINT('',(-0.117775,2.85464118895969E-14,-0.0924367114736175));
#17975=CARTESIAN_POINT('Ctrl Pts',(-0.117590388001671,-3.33269891444124E-5,
1.28256328852638));
#17976=CARTESIAN_POINT('Ctrl Pts',(-0.117634977734708,-0.017625925033684,
1.28374763276543));
#17977=CARTESIAN_POINT('Ctrl Pts',(-0.105676786131388,-0.0744702911817869,
1.28757830688358));
#17978=CARTESIAN_POINT('Ctrl Pts',(-0.0175857351491984,-0.138091953858251,
1.29405531088083));
#17979=CARTESIAN_POINT('Ctrl Pts',(0.106487712804436,-0.089660542174548,
1.30199430051814));
#17980=CARTESIAN_POINT('Ctrl Pts',(0.133078957772855,0.0408489510387311,
1.30993329015544));
#17981=CARTESIAN_POINT('Ctrl Pts',(0.0378455373822902,0.133964029124136,
1.31787227979275));
#17982=CARTESIAN_POINT('Ctrl Pts',(-0.0855601048685178,0.105915403748908,
1.32541561258306));
#17983=CARTESIAN_POINT('Ctrl Pts',(-0.117590074669608,0.0331395035428114,
1.33031261549427));
#17984=CARTESIAN_POINT('Ctrl Pts',(-0.117871679003533,-9.01049542302501E-5,
1.33256328852638));
#17985=CARTESIAN_POINT('Ctrl Pts',(-0.117823716245033,-0.000102811805890825,
1.29243671147362));
#17986=CARTESIAN_POINT('Ctrl Pts',(-0.117892441435953,-0.00760726064997237,
1.29294445975461));
#17987=CARTESIAN_POINT('Ctrl Pts',(-0.113819337750002,-0.0541654333254181,
1.29609959740987));
#17988=CARTESIAN_POINT('Ctrl Pts',(-0.0518146499729274,-0.129225073214149,
1.30190212443939));
#17989=CARTESIAN_POINT('Ctrl Pts',(0.0805213734929343,-0.11357898534207,
1.30984429256217));
#17990=CARTESIAN_POINT('Ctrl Pts',(0.1390915465469,0.0061171215252809,1.31778646068495));
#17991=CARTESIAN_POINT('Ctrl Pts',(0.0702395735793815,0.120209316621791,
1.32572862880773));
#17992=CARTESIAN_POINT('Ctrl Pts',(-0.0629590648350173,0.124177428154433,
1.33367079693051));
#17993=CARTESIAN_POINT('Ctrl Pts',(-0.115917830154768,0.0471875384414626,
1.33924015781913));
#17994=CARTESIAN_POINT('Ctrl Pts',(-0.117945510062545,0.00411888419242175,
1.3421621293335));
#17995=CARTESIAN_POINT('Ctrl Pts',(-0.117917347702326,6.89762296073276E-5,
1.34243671147361));
#17996=CARTESIAN_POINT('Origin',(0.,0.,-0.0924367114736175));
#17997=CARTESIAN_POINT('',(-0.11774949833287,0.000107383800510985,1.23256328852638));
#17998=CARTESIAN_POINT('',(-0.117581795058195,-8.20683476789735E-6,1.24243671147361));
#17999=CARTESIAN_POINT('',(-0.117775,2.85464118895969E-14,-0.0924367114736175));
#18000=CARTESIAN_POINT('Ctrl Pts',(-0.11774949833287,0.000107383800510997,
1.23256328852638));
#18001=CARTESIAN_POINT('Ctrl Pts',(-0.1174869159147,-0.0291008736543001,
1.23453632015749));
#18002=CARTESIAN_POINT('Ctrl Pts',(-0.0917482398636095,-0.0978979247776974,
1.23915568166769));
#18003=CARTESIAN_POINT('Ctrl Pts',(0.0236422145726536,-0.137184880695923,
1.246421373057));
#18004=CARTESIAN_POINT('Ctrl Pts',(0.128082862902196,-0.0545291301253663,
1.2543603626943));
#18005=CARTESIAN_POINT('Ctrl Pts',(0.115272428336817,0.0780443019497631,
1.26229935233161));
#18006=CARTESIAN_POINT('Ctrl Pts',(-0.00306201423577413,0.139173524314926,
1.27023834196891));
#18007=CARTESIAN_POINT('Ctrl Pts',(-0.101358337705897,0.08278581645186,
1.27699298736717));
#18008=CARTESIAN_POINT('Ctrl Pts',(-0.117535345263889,0.02168343817453,
1.28110130288633));
#18009=CARTESIAN_POINT('Ctrl Pts',(-0.117590388001671,-3.33269891444124E-5,
1.28256328852638));
#18010=CARTESIAN_POINT('Ctrl Pts',(-0.117581795058195,-8.20683476789562E-6,
1.24243671147361));
#18011=CARTESIAN_POINT('Ctrl Pts',(-0.117593699448189,-0.0191748937105988,
1.24372679017572));
#18012=CARTESIAN_POINT('Ctrl Pts',(-0.104100832827715,-0.0776580224685839,
1.24766425825208));
#18013=CARTESIAN_POINT('Ctrl Pts',(-0.0120149744006178,-0.138706589206355,
1.25424911570271));
#18014=CARTESIAN_POINT('Ctrl Pts',(0.110059129405696,-0.0852693704304675,
1.26219128382548));
#18015=CARTESIAN_POINT('Ctrl Pts',(0.13130776387206,0.0462833517151888,
1.27013345194827));
#18016=CARTESIAN_POINT('Ctrl Pts',(0.0322649968732001,0.135435768819968,
1.27807562007105));
#18017=CARTESIAN_POINT('Ctrl Pts',(-0.0881142830049797,0.102747609761224,
1.28551003991283));
#18018=CARTESIAN_POINT('Ctrl Pts',(-0.117534109666069,0.0315207854174475,
1.29029707038035));
#18019=CARTESIAN_POINT('Ctrl Pts',(-0.117823716245033,-0.000102811805890825,
1.29243671147362));
#18020=CARTESIAN_POINT('Origin',(0.,0.,-0.0924367114736175));
#18021=CARTESIAN_POINT('',(-0.117957988745754,-3.12301727557783E-5,1.18256328852638));
#18022=CARTESIAN_POINT('',(-0.117793553451004,0.000106755881474893,1.19243671147362));
#18023=CARTESIAN_POINT('',(-0.117775,2.85464118895969E-14,-0.0924367114736175));
#18024=CARTESIAN_POINT('Ctrl Pts',(-0.117957988745754,-3.12301727557569E-5,
1.18256328852638));
#18025=CARTESIAN_POINT('Ctrl Pts',(-0.117964007145535,-0.00173159226684161,
1.18267867767044));
#18026=CARTESIAN_POINT('Ctrl Pts',(-0.117160216762375,-0.0424221720604921,
1.1854403966936));
#18027=CARTESIAN_POINT('Ctrl Pts',(-0.0703321751825429,-0.12013338809653,
1.19084844559586));
#18028=CARTESIAN_POINT('Ctrl Pts',(0.0627954496153871,-0.124239193932754,
1.19878743523316));
#18029=CARTESIAN_POINT('Ctrl Pts',(0.138438143943654,-0.0146125323915816,
1.20672642487047));
#18030=CARTESIAN_POINT('Ctrl Pts',(0.0873502052771435,0.108390901091839,
1.21466541450777));
#18031=CARTESIAN_POINT('Ctrl Pts',(-0.043700859820065,0.132169893139269,
1.22260440414508));
#18032=CARTESIAN_POINT('Ctrl Pts',(-0.112119660921406,0.0591163174148552,
1.22857036215128));
#18033=CARTESIAN_POINT('Ctrl Pts',(-0.117839104743291,0.0100747194789664,
1.23188999027838));
#18034=CARTESIAN_POINT('Ctrl Pts',(-0.11774949833287,0.000107383800510997,
1.23256328852638));
#18035=CARTESIAN_POINT('Ctrl Pts',(-0.117793553451004,0.000106755881474891,
1.19243671147362));
#18036=CARTESIAN_POINT('Ctrl Pts',(-0.117510050331475,-0.0305433296418112,
1.19450912059683));
#18037=CARTESIAN_POINT('Ctrl Pts',(-0.0896091397727994,-0.100804620014092,
1.19922891909429));
#18038=CARTESIAN_POINT('Ctrl Pts',(0.0288222657999454,-0.136209964735594,
1.20659610696603));
#18039=CARTESIAN_POINT('Ctrl Pts',(0.130092623711363,-0.0495962373069701,
1.21453827508881));
#18040=CARTESIAN_POINT('Ctrl Pts',(0.112184773380136,0.082452738709893,
1.22248044321158));
#18041=CARTESIAN_POINT('Ctrl Pts',(-0.00849585454694533,0.138966535376798,
1.23042261133437));
#18042=CARTESIAN_POINT('Ctrl Pts',(-0.103054997843392,0.079672038485689,
1.23707470075504));
#18043=CARTESIAN_POINT('Ctrl Pts',(-0.11756927027536,0.0201573447738481,
1.24107940080146));
#18044=CARTESIAN_POINT('Ctrl Pts',(-0.117581795058195,-8.20683476789562E-6,
1.24243671147361));
#18045=CARTESIAN_POINT('Origin',(0.,0.,-0.0924367114736175));
#18046=CARTESIAN_POINT('',(-0.117657565919426,-8.78585414499747E-5,1.13256328852638));
#18047=CARTESIAN_POINT('',(-0.117937823388479,-5.4172489969917E-5,1.14243671147362));
#18048=CARTESIAN_POINT('',(-0.117775,2.85464118895969E-14,-0.0924367114736175));
#18049=CARTESIAN_POINT('Ctrl Pts',(-0.117657565919426,-8.78585414499974E-5,
1.13256328852638));
#18050=CARTESIAN_POINT('Ctrl Pts',(-0.11775046973706,-0.0134980674796043,
1.13346736506249));
#18051=CARTESIAN_POINT('Ctrl Pts',(-0.109441032251172,-0.0660497484721492,
1.13701777147771));
#18052=CARTESIAN_POINT('Ctrl Pts',(-0.0320511128216771,-0.13546723577438,
1.14321450777202));
#18053=CARTESIAN_POINT('Ctrl Pts',(0.0964380908528195,-0.100390938007982,
1.15115349740933));
#18054=CARTESIAN_POINT('Ctrl Pts',(0.136644831685568,0.0265863832644056,
1.15909248704664));
#18055=CARTESIAN_POINT('Ctrl Pts',(0.0517625939920979,0.129225692742072,
1.16703147668394));
#18056=CARTESIAN_POINT('Ctrl Pts',(-0.0785823129332351,0.113795317289389,
1.17485507717719));
#18057=CARTESIAN_POINT('Ctrl Pts',(-0.117825981412732,0.0372644419932696,
1.18003234779134));
#18058=CARTESIAN_POINT('Ctrl Pts',(-0.117957988745754,-3.12301727557569E-5,
1.18256328852638));
#18059=CARTESIAN_POINT('Ctrl Pts',(-0.117937823388479,-5.41724899699178E-5,
1.14243671147362));
#18060=CARTESIAN_POINT('Ctrl Pts',(-0.117955293269658,-0.0031110520517566,
1.14264406164367));
#18061=CARTESIAN_POINT('Ctrl Pts',(-0.116460933142332,-0.0451799670343263,
1.14549880118799));
#18062=CARTESIAN_POINT('Ctrl Pts',(-0.0660858892268601,-0.122541963197144,
1.15100093010657));
#18063=CARTESIAN_POINT('Ctrl Pts',(0.0671705316110708,-0.121950798202395,
1.15894309822935));
#18064=CARTESIAN_POINT('Ctrl Pts',(0.138891844802359,-0.00964017357273747,
1.16688526635212));
#18065=CARTESIAN_POINT('Ctrl Pts',(0.0833739592533277,0.111501840422208,
1.17482743447491));
#18066=CARTESIAN_POINT('Ctrl Pts',(-0.0485230383040216,0.130496713571114,
1.18276960259768));
#18067=CARTESIAN_POINT('Ctrl Pts',(-0.113150295826959,0.0561813708375219,
1.18863936159726));
#18068=CARTESIAN_POINT('Ctrl Pts',(-0.117872210070015,0.00861047923971886,
1.19186173122257));
#18069=CARTESIAN_POINT('Ctrl Pts',(-0.117793553451004,0.000106755881474891,
1.19243671147362));
#18070=CARTESIAN_POINT('Origin',(0.,0.,-0.0924367114736175));
#18071=CARTESIAN_POINT('',(-0.117641451221435,8.0229283111194E-5,1.08256328852638));
#18072=CARTESIAN_POINT('',(-0.117630591849015,-7.42484764288953E-5,1.09243671147362));
#18073=CARTESIAN_POINT('',(-0.117775,2.85464118895969E-14,-0.0924367114736175));
#18074=CARTESIAN_POINT('Ctrl Pts',(-0.117641451221435,8.02292831111745E-5,
1.08256328852638));
#18075=CARTESIAN_POINT('Ctrl Pts',(-0.117483998834985,-0.0250372639622414,
1.08425605245455));
#18076=CARTESIAN_POINT('Ctrl Pts',(-0.0972946570053161,-0.0896524615425008,
1.08859514626182));
#18077=CARTESIAN_POINT('Ctrl Pts',(0.00904258428980543,-0.13891320121148,
1.09558056994819));
#18078=CARTESIAN_POINT('Ctrl Pts',(0.121617839487272,-0.067732908692211,
1.1035195595855));
#18079=CARTESIAN_POINT('Ctrl Pts',(0.122860297649024,0.0654522196953821,
1.1114585492228));
#18080=CARTESIAN_POINT('Ctrl Pts',(0.0116325734791967,0.138720326685422,
1.11939753886011));
#18081=CARTESIAN_POINT('Ctrl Pts',(-0.096364912740844,0.0911171059582243,
1.1264324519613));
#18082=CARTESIAN_POINT('Ctrl Pts',(-0.117478530206868,0.0257550656131636,
1.13082103518339));
#18083=CARTESIAN_POINT('Ctrl Pts',(-0.117657565919426,-8.78585414499974E-5,
1.13256328852638));
#18084=CARTESIAN_POINT('Ctrl Pts',(-0.117630591849015,-7.42484764288814E-5,
1.09243671147362));
#18085=CARTESIAN_POINT('Ctrl Pts',(-0.117715241483118,-0.0147626739157663,
1.09342639206478));
#18086=CARTESIAN_POINT('Ctrl Pts',(-0.108350501834675,-0.0686384992808382,
1.0970634620302));
#18087=CARTESIAN_POINT('Ctrl Pts',(-0.0276126195379174,-0.136460326620484,
1.10334792136989));
#18088=CARTESIAN_POINT('Ctrl Pts',(0.0997182217817603,-0.0971604536002107,
1.11129008949267));
#18089=CARTESIAN_POINT('Ctrl Pts',(0.135696927507188,0.0311483765905046,
1.11923225761545));
#18090=CARTESIAN_POINT('Ctrl Pts',(0.0473633069609982,0.130922093830007,
1.12717442573822));
#18091=CARTESIAN_POINT('Ctrl Pts',(-0.0809210029008042,0.111284164335459,
1.13490924369095));
#18092=CARTESIAN_POINT('Ctrl Pts',(-0.117732242679493,0.0359183370635313,
1.13999667226941));
#18093=CARTESIAN_POINT('Ctrl Pts',(-0.117937823388479,-5.41724899699178E-5,
1.14243671147362));
#18094=CARTESIAN_POINT('Origin',(0.,0.,-0.0924367114736175));
#18095=CARTESIAN_POINT('',(-0.117948158721073,4.38502512853227E-5,1.03256328852638));
#18096=CARTESIAN_POINT('',(-0.117667547954054,9.20194976846214E-5,1.04243671147362));
#18097=CARTESIAN_POINT('',(-0.117775,2.85464118895969E-14,-0.0924367114736175));
#18098=CARTESIAN_POINT('Ctrl Pts',(-0.117948158721073,4.38502512853157E-5,
1.03256328852638));
#18099=CARTESIAN_POINT('Ctrl Pts',(-0.117773439871091,-0.0365306738650768,
1.03504473984661));
#18100=CARTESIAN_POINT('Ctrl Pts',(-0.0798690478914953,-0.112422454385097,
1.04017252104593));
#18101=CARTESIAN_POINT('Ctrl Pts',(0.0493427524230464,-0.130168884856471,
1.04794663212436));
#18102=CARTESIAN_POINT('Ctrl Pts',(0.136125055048066,-0.0291310004912345,
1.05588562176166));
#18103=CARTESIAN_POINT('Ctrl Pts',(0.0982941990358779,0.0985743183458784,
1.06382461139897));
#18104=CARTESIAN_POINT('Ctrl Pts',(-0.0295182596522469,0.136041604476578,
1.07176360103627));
#18105=CARTESIAN_POINT('Ctrl Pts',(-0.108818061611988,0.067537217334308,
1.07800982674541));
#18106=CARTESIAN_POINT('Ctrl Pts',(-0.11773014713001,0.0142293884972668,
1.08160972257545));
#18107=CARTESIAN_POINT('Ctrl Pts',(-0.117641451221435,8.02292831111745E-5,
1.08256328852638));
#18108=CARTESIAN_POINT('Ctrl Pts',(-0.117667547954054,9.20194976846197E-5,
1.04243671147362));
#18109=CARTESIAN_POINT('Ctrl Pts',(-0.117475882803567,-0.0261866690710452,
1.04420872248589));
#18110=CARTESIAN_POINT('Ctrl Pts',(-0.0957916308421219,-0.0920126959480487,
1.04862812287242));
#18111=CARTESIAN_POINT('Ctrl Pts',(0.0132451643780021,-0.13859452774087,
1.05569491263321));
#18112=CARTESIAN_POINT('Ctrl Pts',(0.123654649330263,-0.0639797248987874,
1.06363708075599));
#18113=CARTESIAN_POINT('Ctrl Pts',(0.120783771971213,0.0692470788374567,
1.07157924887876));
#18114=CARTESIAN_POINT('Ctrl Pts',(0.00726255089817806,0.139036444335888,
1.07952141700155));
#18115=CARTESIAN_POINT('Ctrl Pts',(-0.0979368667310299,0.0886295245336828,
1.08647390453316));
#18116=CARTESIAN_POINT('Ctrl Pts',(-0.117488804242801,0.0245287720112504,
1.09077900269052));
#18117=CARTESIAN_POINT('Ctrl Pts',(-0.117630591849015,-7.42484764288814E-5,
1.09243671147362));
#18118=CARTESIAN_POINT('Origin',(0.,0.,-0.0924367114736175));
#18119=CARTESIAN_POINT('',(-0.117771476475648,-0.000107683352847938,0.982563288526384));
#18120=CARTESIAN_POINT('',(-0.11796176292438,2.53781033017321E-5,0.992436711473616));
#18121=CARTESIAN_POINT('',(-0.117775,2.85464118895969E-14,-0.0924367114736175));
#18122=CARTESIAN_POINT('Ctrl Pts',(-0.117771476475648,-0.000107683352847945,
0.982563288526384));
#18123=CARTESIAN_POINT('Ctrl Pts',(-0.117856103358663,-0.00933799346614349,
0.983187097359559));
#18124=CARTESIAN_POINT('Ctrl Pts',(-0.112646870919438,-0.057630810124202,
0.986457236071836));
#18125=CARTESIAN_POINT('Ctrl Pts',(-0.0461590140787468,-0.131331607851033,
0.992373704663214));
#18126=CARTESIAN_POINT('Ctrl Pts',(0.0853128637208732,-0.110001641284132,
1.00031269430052));
#18127=CARTESIAN_POINT('Ctrl Pts',(0.138686661656432,0.0120272889735618,
1.00825168393783));
#18128=CARTESIAN_POINT('Ctrl Pts',(0.0651023256631918,0.123046060459907,
1.01619067357513));
#18129=CARTESIAN_POINT('Ctrl Pts',(-0.0680787277209358,0.121424596492465,
1.02412966321244));
#18130=CARTESIAN_POINT('Ctrl Pts',(-0.116790117880403,0.0438975063746073,
1.02958720152952));
#18131=CARTESIAN_POINT('Ctrl Pts',(-0.11795976781127,0.00247402277930658,
1.0323984099675));
#18132=CARTESIAN_POINT('Ctrl Pts',(-0.117948158721073,4.38502512853157E-5,
1.03256328852638));
#18133=CARTESIAN_POINT('Ctrl Pts',(-0.11796176292438,2.53781033017319E-5,
0.992436711473616));
#18134=CARTESIAN_POINT('Ctrl Pts',(-0.117851518882229,-0.0376119105440478,
0.994991052906992));
#18135=CARTESIAN_POINT('Ctrl Pts',(-0.077958511321084,-0.114458475672252,
1.00019278371463));
#18136=CARTESIAN_POINT('Ctrl Pts',(0.0529591494285269,-0.128760265574912,
1.00804190389653));
#18137=CARTESIAN_POINT('Ctrl Pts',(0.136912761112491,-0.0252739657289669,
1.0159840720193));
#18138=CARTESIAN_POINT('Ctrl Pts',(0.0954402180350474,0.101365883217864,
1.02392624014209));
#18139=CARTESIAN_POINT('Ctrl Pts',(-0.0334653697086341,0.135144169424284,
1.03186840826486));
#18140=CARTESIAN_POINT('Ctrl Pts',(-0.109792739119276,0.0652029671457737,
1.03803856537538));
#18141=CARTESIAN_POINT('Ctrl Pts',(-0.117762231070763,0.0130737646421874,
1.04156133311163));
#18142=CARTESIAN_POINT('Ctrl Pts',(-0.117667547954054,9.20194976846197E-5,
1.04243671147362));
#18143=CARTESIAN_POINT('Origin',(0.,0.,-0.0924367114736175));
#18144=CARTESIAN_POINT('',(-0.117585265278523,2.16484251076657E-5,0.932563288526384));
#18145=CARTESIAN_POINT('',(-0.117742563953077,-0.000107211314308964,0.942436711473616));
#18146=CARTESIAN_POINT('',(-0.117775,2.85464118895969E-14,-0.0924367114736175));
#18147=CARTESIAN_POINT('Ctrl Pts',(-0.117585265278523,2.16484251076635E-5,
0.932563288526384));
#18148=CARTESIAN_POINT('Ctrl Pts',(-0.117550805757046,-0.0209622679161363,
0.933975784751614));
#18149=CARTESIAN_POINT('Ctrl Pts',(-0.102172791552808,-0.0813069697478888,
0.938034610855947));
#18150=CARTESIAN_POINT('Ctrl Pts',(-0.00565790085648466,-0.139092177922979,
0.944739766839381));
#18151=CARTESIAN_POINT('Ctrl Pts',(0.113796373024222,-0.0801812402497705,
0.952678756476687));
#18152=CARTESIAN_POINT('Ctrl Pts',(0.129077866376032,0.0521301276928276,
0.960617746113992));
#18153=CARTESIAN_POINT('Ctrl Pts',(0.026197419344502,0.13671993644362,0.968556735751298));
#18154=CARTESIAN_POINT('Ctrl Pts',(-0.0906967139502387,0.0993396518733501,
0.975871916555428));
#18155=CARTESIAN_POINT('Ctrl Pts',(-0.117497098103867,0.02981894716558,
0.980540767480457));
#18156=CARTESIAN_POINT('Ctrl Pts',(-0.117771476475648,-0.000107683352847945,
0.982563288526384));
#18157=CARTESIAN_POINT('Ctrl Pts',(-0.117742563953077,-0.000107211314308957,
0.942436711473616));
#18158=CARTESIAN_POINT('Ctrl Pts',(-0.117833632602859,-0.0103126986533654,
0.943125993953839));
#18159=CARTESIAN_POINT('Ctrl Pts',(-0.111944766202914,-0.0596118697348184,
0.946462665808322));
#18160=CARTESIAN_POINT('Ctrl Pts',(-0.0428565117498991,-0.132465832952297,
0.952446727037066));
#18161=CARTESIAN_POINT('Ctrl Pts',(0.0880997963686447,-0.107806787258123,
0.960388895159846));
#18162=CARTESIAN_POINT('Ctrl Pts',(0.138347640177547,0.0156143509765511,
0.968331063282625));
#18163=CARTESIAN_POINT('Ctrl Pts',(0.061854832590724,0.124731139593481,
0.976273231405407));
#18164=CARTESIAN_POINT('Ctrl Pts',(-0.0713033562375951,0.119581390225944,
0.984215399528185));
#18165=CARTESIAN_POINT('Ctrl Pts',(-0.117322772537986,0.0417718924351975,
0.989603226217589));
#18166=CARTESIAN_POINT('Ctrl Pts',(-0.11796577882491,0.00139640554830399,
0.992343663532733));
#18167=CARTESIAN_POINT('Ctrl Pts',(-0.11796176292438,2.53781033017319E-5,
0.992436711473616));
#18168=CARTESIAN_POINT('Origin',(0.,0.,-0.0924367114736175));
#18169=CARTESIAN_POINT('',(-0.117850913371472,9.6525574830472E-5,0.882563288526384));
#18170=CARTESIAN_POINT('',(-0.117591231449503,3.54948526558943E-5,0.892436711473616));
#18171=CARTESIAN_POINT('',(-0.117775,2.85464118895969E-14,-0.0924367114736175));
#18172=CARTESIAN_POINT('Ctrl Pts',(-0.117850913371472,9.65255748304767E-5,
0.882563288526384));
#18173=CARTESIAN_POINT('Ctrl Pts',(-0.117563006813672,-0.0324172738354332,
0.884764472143669));
#18174=CARTESIAN_POINT('Ctrl Pts',(-0.0867151192651892,-0.104499852648429,
0.889611985640057));
#18175=CARTESIAN_POINT('Ctrl Pts',(0.0353397195745277,-0.134646760160997,
0.897105829015547));
#18176=CARTESIAN_POINT('Ctrl Pts',(0.132293719443212,-0.0433245611326863,
0.905044818652852));
#18177=CARTESIAN_POINT('Ctrl Pts',(0.108141885842356,0.0876583043865096,
0.912983808290157));
#18178=CARTESIAN_POINT('Ctrl Pts',(-0.0150064327997127,0.138395999855801,
0.920922797927463));
#18179=CARTESIAN_POINT('Ctrl Pts',(-0.104951114476159,0.0759553573435841,
0.927449291339539));
#18180=CARTESIAN_POINT('Ctrl Pts',(-0.117615366114572,0.01835136974357,
0.931329454872513));
#18181=CARTESIAN_POINT('Ctrl Pts',(-0.117585265278523,2.16484251076635E-5,
0.932563288526384));
#18182=CARTESIAN_POINT('Ctrl Pts',(-0.117591231449503,3.54948526559117E-5,
0.892436711473616));
#18183=CARTESIAN_POINT('Ctrl Pts',(-0.117532234588281,-0.0218238662162972,
0.893908324374946));
#18184=CARTESIAN_POINT('Ctrl Pts',(-0.101194437785642,-0.0830895288483654,
0.898027326650536));
#18185=CARTESIAN_POINT('Ctrl Pts',(-0.00250162451743248,-0.139203517821528,
0.904793718300386));
#18186=CARTESIAN_POINT('Ctrl Pts',(0.115632500949424,-0.0775435504945224,
0.912735886423165));
#18187=CARTESIAN_POINT('Ctrl Pts',(0.127835376168433,0.0551542754370876,
0.920678054545947));
#18188=CARTESIAN_POINT('Ctrl Pts',(0.0229279137899797,0.137325118854324,
0.928620222668725));
#18189=CARTESIAN_POINT('Ctrl Pts',(-0.0920562790907298,0.0974788594069619,
0.935873108311283));
#18190=CARTESIAN_POINT('Ctrl Pts',(-0.117483857027998,0.0288844367965532,
0.94047860457958));
#18191=CARTESIAN_POINT('Ctrl Pts',(-0.117742563953077,-0.000107211314308957,
0.942436711473616));
#18192=CARTESIAN_POINT('Origin',(0.,0.,-0.0924367114736175));
#18193=CARTESIAN_POINT('',(-0.11789232318732,-8.18790992476613E-5,0.832563288526384));
#18194=CARTESIAN_POINT('',(-0.117872825429845,8.99519344067963E-5,0.842436711473616));
#18195=CARTESIAN_POINT('',(-0.117775,2.85464118895969E-14,-0.0924367114736175));
#18196=CARTESIAN_POINT('Ctrl Pts',(-0.11789232318732,-8.18790992476734E-5,
0.832563288526384));
#18197=CARTESIAN_POINT('Ctrl Pts',(-0.117932494517479,-0.00515170743829337,
0.832906829656623));
#18198=CARTESIAN_POINT('Ctrl Pts',(-0.115332713682068,-0.0492334187378749,
0.835896700665964));
#18199=CARTESIAN_POINT('Ctrl Pts',(-0.059752088941783,-0.125731196083361,
0.841532901554406));
#18200=CARTESIAN_POINT('Ctrl Pts',(0.0732361146625898,-0.118385460722959,
0.849471891191712));
#18201=CARTESIAN_POINT('Ctrl Pts',(0.139181674492094,-0.00266594955618734,
0.857410880829018));
#18202=CARTESIAN_POINT('Ctrl Pts',(0.077715950067195,0.115494055719818,
0.865349870466323));
#18203=CARTESIAN_POINT('Ctrl Pts',(-0.0548934004223171,0.127927168308903,
0.87328886010363));
#18204=CARTESIAN_POINT('Ctrl Pts',(-0.114416768398411,0.0522742940766184,
0.879026666123649));
#18205=CARTESIAN_POINT('Ctrl Pts',(-0.117909136832228,0.0066718045071592,
0.882118142264567));
#18206=CARTESIAN_POINT('Ctrl Pts',(-0.117850913371472,9.65255748304767E-5,
0.882563288526384));
#18207=CARTESIAN_POINT('Ctrl Pts',(-0.117872825429845,8.99519344067998E-5,
0.842436711473616));
#18208=CARTESIAN_POINT('Ctrl Pts',(-0.117591169542271,-0.0331870933343037,
0.844690654796053));
#18209=CARTESIAN_POINT('Ctrl Pts',(-0.0854771005934613,-0.106025606004136,
0.84959198749275));
#18210=CARTESIAN_POINT('Ctrl Pts',(0.0380692928980519,-0.133920149482284,
0.857140709563706));
#18211=CARTESIAN_POINT('Ctrl Pts',(0.133179650076608,-0.0405839661022353,
0.865082877686486));
#18212=CARTESIAN_POINT('Ctrl Pts',(0.106283765719693,0.0899312995767124,
0.873025045809266));
#18213=CARTESIAN_POINT('Ctrl Pts',(-0.0179789669825735,0.138060255849953,
0.880967213932046));
#18214=CARTESIAN_POINT('Ctrl Pts',(-0.105798194743126,0.0742290978659706,
0.887437769153496));
#18215=CARTESIAN_POINT('Ctrl Pts',(-0.117638368248411,0.0175004969839459,
0.891260935000686));
#18216=CARTESIAN_POINT('Ctrl Pts',(-0.117591231449503,3.54948526559117E-5,
0.892436711473616));
#18217=CARTESIAN_POINT('Origin',(0.,0.,-0.0924367114736175));
#18218=CARTESIAN_POINT('',(-0.117598114366551,-4.51832715892789E-5,0.782563288526384));
#18219=CARTESIAN_POINT('',(-0.117874685330111,-8.92836445515327E-5,0.792436711473617));
#18220=CARTESIAN_POINT('',(-0.117775,2.85464118895969E-14,-0.0924367114736175));
#18221=CARTESIAN_POINT('Ctrl Pts',(-0.117598114366551,-4.518327158929E-5,
0.782563288526384));
#18222=CARTESIAN_POINT('Ctrl Pts',(-0.117656123976761,-0.0168608793038394,
0.783695517048678));
#18223=CARTESIAN_POINT('Ctrl Pts',(-0.106420815930739,-0.0729055463807818,
0.787474075450074));
#18224=CARTESIAN_POINT('Ctrl Pts',(-0.0202952816069424,-0.137719814645367,
0.793898963730571));
#18225=CARTESIAN_POINT('Ctrl Pts',(0.104705698854998,-0.0917352845351548,
0.801837953367879));
#18226=CARTESIAN_POINT('Ctrl Pts',(0.133855787965376,0.0382266115373486,
0.809776943005182));
#18227=CARTESIAN_POINT('Ctrl Pts',(0.0404700769297216,0.133194664588195,
0.81771593264249));
#18228=CARTESIAN_POINT('Ctrl Pts',(-0.0843190215395119,0.107398870964955,
0.825311381149555));
#18229=CARTESIAN_POINT('Ctrl Pts',(-0.117623050954756,0.0339016606582783,
0.830260499777521));
#18230=CARTESIAN_POINT('Ctrl Pts',(-0.11789232318732,-8.18790992476734E-5,
0.832563288526384));
#18231=CARTESIAN_POINT('Ctrl Pts',(-0.117874685330111,-8.9283644551537E-5,
0.792436711473617));
#18232=CARTESIAN_POINT('Ctrl Pts',(-0.11792303416021,-0.00583050672374999,
0.7928255958429));
#18233=CARTESIAN_POINT('Ctrl Pts',(-0.114931453360353,-0.0506053896743902,
0.795861869586443));
#18234=CARTESIAN_POINT('Ctrl Pts',(-0.0575513573065257,-0.126774282767806,
0.801545532704245));
#18235=CARTESIAN_POINT('Ctrl Pts',(0.0753527000357912,-0.117071978271622,
0.809487700827026));
#18236=CARTESIAN_POINT('Ctrl Pts',(0.139225942868322,-0.000119714417332432,
0.817429868949805));
#18237=CARTESIAN_POINT('Ctrl Pts',(0.0755539188089132,0.116942220141962,
0.825372037072586));
#18238=CARTESIAN_POINT('Ctrl Pts',(-0.0573332568284509,0.12687306712048,
0.833314205195366));
#18239=CARTESIAN_POINT('Ctrl Pts',(-0.114890414736801,0.0507419104293215,
0.839002429995709));
#18240=CARTESIAN_POINT('Ctrl Pts',(-0.117921990994851,0.00589875908008548,
0.842043265421793));
#18241=CARTESIAN_POINT('Ctrl Pts',(-0.117872825429845,8.99519344067998E-5,
0.842436711473616));
#18242=CARTESIAN_POINT('Origin',(0.,0.,-0.0924367114736175));
#18243=CARTESIAN_POINT('',(-0.11772691567491,0.000105512987197037,0.732563288526384));
#18244=CARTESIAN_POINT('',(-0.117591850253004,-3.65476421498312E-5,0.742436711473616));
#18245=CARTESIAN_POINT('',(-0.117775,2.85464118895969E-14,-0.0924367114736175));
#18246=CARTESIAN_POINT('Ctrl Pts',(-0.11772691567491,0.000105512987197042,
0.732563288526384));
#18247=CARTESIAN_POINT('Ctrl Pts',(-0.117479624464894,-0.0283451130369189,
0.734484204440733));
#18248=CARTESIAN_POINT('Ctrl Pts',(-0.0928318426870313,-0.096374559506161,
0.739051450234184));
#18249=CARTESIAN_POINT('Ctrl Pts',(0.0209425314183671,-0.137622876656644,
0.746265025906738));
#18250=CARTESIAN_POINT('Ctrl Pts',(0.126986869252672,-0.0570349089493802,
0.754204015544043));
#18251=CARTESIAN_POINT('Ctrl Pts',(0.11678343126468,0.0757646090434518,
0.762143005181349));
#18252=CARTESIAN_POINT('Ctrl Pts',(-0.000327234354877375,0.139206819944772,
0.770081994818654));
#18253=CARTESIAN_POINT('Ctrl Pts',(-0.100479183608201,0.0843410365921374,
0.776888755933667));
#18254=CARTESIAN_POINT('Ctrl Pts',(-0.117520539541507,0.0224420334666934,
0.781049187169576));
#18255=CARTESIAN_POINT('Ctrl Pts',(-0.117598114366551,-4.518327158929E-5,
0.782563288526384));
#18256=CARTESIAN_POINT('Ctrl Pts',(-0.117591850253004,-3.65476421498364E-5,
0.742436711473616));
#18257=CARTESIAN_POINT('Ctrl Pts',(-0.117640211257931,-0.0174335619022046,
0.743607926264006));
#18258=CARTESIAN_POINT('Ctrl Pts',(-0.105863856762799,-0.0740921523660566,
0.747426530428656));
#18259=CARTESIAN_POINT('Ctrl Pts',(-0.0182163644075178,-0.138029133036789,
0.753892523967566));
#18260=CARTESIAN_POINT('Ctrl Pts',(0.106128952536144,-0.0901139441634624,
0.761834692090347));
#18261=CARTESIAN_POINT('Ctrl Pts',(0.133249245915149,0.0403548753208232,
0.769776860213125));
#18262=CARTESIAN_POINT('Ctrl Pts',(0.0382995408207276,0.133854483197375,
0.777719028335907));
#18263=CARTESIAN_POINT('Ctrl Pts',(-0.0853693283863186,0.106155717082476,
0.785272312089402));
#18264=CARTESIAN_POINT('Ctrl Pts',(-0.117593892160246,0.0332537408718532,
0.79017820646864));
#18265=CARTESIAN_POINT('Ctrl Pts',(-0.117874685330111,-8.9283644551537E-5,
0.792436711473617));
#18266=CARTESIAN_POINT('Origin',(0.,0.,-0.0924367114736175));
#18267=CARTESIAN_POINT('',(-0.117964947617991,-1.73329198795185E-5,0.682563288526384));
#18268=CARTESIAN_POINT('',(-0.117740574064672,0.000107068518266168,0.692436711473616));
#18269=CARTESIAN_POINT('',(-0.117775,2.85464118895969E-14,-0.0924367114736175));
#18270=CARTESIAN_POINT('Ctrl Pts',(-0.117964947617991,-1.73329198795367E-5,
0.682563288526384));
#18271=CARTESIAN_POINT('Ctrl Pts',(-0.117966864156947,-0.000949576032666658,
0.682626561953687));
#18272=CARTESIAN_POINT('Ctrl Pts',(-0.117534558560489,-0.0408698671952461,
0.685336165260092));
#18273=CARTESIAN_POINT('Ctrl Pts',(-0.0726787294560835,-0.118728463672822,
0.690692098445597));
#18274=CARTESIAN_POINT('Ctrl Pts',(0.0603425395611779,-0.125448888878168,
0.698631088082904));
#18275=CARTESIAN_POINT('Ctrl Pts',(0.138124349154501,-0.0173294538893964,
0.706570077720209));
#18276=CARTESIAN_POINT('Ctrl Pts',(0.0894627833767505,0.106653908470079,
0.714509067357515));
#18277=CARTESIAN_POINT('Ctrl Pts',(-0.0410958292974484,0.133002927094911,
0.72244805699482));
#18278=CARTESIAN_POINT('Ctrl Pts',(-0.111546724107196,0.0606813038481789,
0.728466130717777));
#18279=CARTESIAN_POINT('Ctrl Pts',(-0.117820302634623,0.0108495967181263,
0.731837874561632));
#18280=CARTESIAN_POINT('Ctrl Pts',(-0.11772691567491,0.000105512987197042,
0.732563288526384));
#18281=CARTESIAN_POINT('Ctrl Pts',(-0.117740574064672,0.000107068518266165,
0.692436711473616));
#18282=CARTESIAN_POINT('Ctrl Pts',(-0.117483171888848,-0.0288182833237499,
0.694390256685113));
#18283=CARTESIAN_POINT('Ctrl Pts',(-0.0921515028359353,-0.0973455904149804,
0.698991191270869));
#18284=CARTESIAN_POINT('Ctrl Pts',(0.022691720100341,-0.137364345221032,
0.706239515230886));
#18285=CARTESIAN_POINT('Ctrl Pts',(0.127740337615313,-0.0553740340325759,
0.714181683353665));
#18286=CARTESIAN_POINT('Ctrl Pts',(0.115765682611161,0.077344581120379,
0.722123851476446));
#18287=CARTESIAN_POINT('Ctrl Pts',(-0.00226223072526165,0.139207614056346,
0.730066019599226));
#18288=CARTESIAN_POINT('Ctrl Pts',(-0.101117998472899,0.083225715609228,
0.736836972931616));
#18289=CARTESIAN_POINT('Ctrl Pts',(-0.117530897055598,0.0218902846491045,
0.740960536889746));
#18290=CARTESIAN_POINT('Ctrl Pts',(-0.117591850253004,-3.65476421498364E-5,
0.742436711473616));
#18291=CARTESIAN_POINT('Origin',(0.,0.,-0.0924367114736175));
#18292=CARTESIAN_POINT('',(-0.117676160015555,-9.46906955630148E-5,0.632563288526383));
#18293=CARTESIAN_POINT('',(-0.117962383120995,-2.41598447144192E-5,0.642436711473616));
#18294=CARTESIAN_POINT('',(-0.117775,2.85464118895969E-14,-0.0924367114736175));
#18295=CARTESIAN_POINT('Ctrl Pts',(-0.117676160015555,-9.46906955630045E-5,
0.632563288526383));
#18296=CARTESIAN_POINT('Ctrl Pts',(-0.117771520970562,-0.0127268345011372,
0.633415249345741));
#18297=CARTESIAN_POINT('Ctrl Pts',(-0.110078248258936,-0.064483421762156,
0.636913540044201));
#18298=CARTESIAN_POINT('Ctrl Pts',(-0.0347063025259737,-0.134811417789573,
0.643058160621763));
#18299=CARTESIAN_POINT('Ctrl Pts',(0.0944472082050275,-0.102266175560326,
0.65099715025907));
#18300=CARTESIAN_POINT('Ctrl Pts',(0.137140772714236,0.0238967416356601,
0.658936139896373));
#18301=CARTESIAN_POINT('Ctrl Pts',(0.054291358674537,0.128183829614862,
0.666875129533682));
#18302=CARTESIAN_POINT('Ctrl Pts',(-0.0772016597727435,0.11523146575827,
0.674750845743682));
#18303=CARTESIAN_POINT('Ctrl Pts',(-0.117886707375211,0.0380402955314478,
0.679980232074585));
#18304=CARTESIAN_POINT('Ctrl Pts',(-0.117964947617991,-1.73329198795367E-5,
0.682563288526384));
#18305=CARTESIAN_POINT('Ctrl Pts',(-0.117962383120995,-2.41598447144253E-5,
0.642436711473616));
#18306=CARTESIAN_POINT('Ctrl Pts',(-0.117966033213387,-0.0013279541977536,
0.642525197731959));
#18307=CARTESIAN_POINT('Ctrl Pts',(-0.117355585052125,-0.0416360146359673,
0.645261073364563));
#18308=CARTESIAN_POINT('Ctrl Pts',(-0.0715088964667609,-0.119458592094588,
0.650644338371427));
#18309=CARTESIAN_POINT('Ctrl Pts',(0.0616402393688536,-0.124837327709565,
0.658586506494205));
#18310=CARTESIAN_POINT('Ctrl Pts',(0.138320583400205,-0.0158522461166236,
0.666528674616987));
#18311=CARTESIAN_POINT('Ctrl Pts',(0.0882850628235238,0.107655121482266,
0.674470842739765));
#18312=CARTESIAN_POINT('Ctrl Pts',(-0.0426286451686149,0.132539337972556,
0.682413010862546));
#18313=CARTESIAN_POINT('Ctrl Pts',(-0.111894847147975,0.059748848130285,
0.68840163377383));
#18314=CARTESIAN_POINT('Ctrl Pts',(-0.117831996057943,0.0103805377030848,
0.691742867310853));
#18315=CARTESIAN_POINT('Ctrl Pts',(-0.117740574064672,0.000107068518266165,
0.692436711473616));
#18316=CARTESIAN_POINT('Origin',(0.,0.,-0.0924367114736175));
#18317=CARTESIAN_POINT('',(-0.117626285855324,7.11112359239178E-5,0.582563288526384));
#18318=CARTESIAN_POINT('',(-0.11766919235599,-9.26074537421634E-5,0.592436711473616));
#18319=CARTESIAN_POINT('',(-0.117775,2.85464118895969E-14,-0.0924367114736175));
#18320=CARTESIAN_POINT('Ctrl Pts',(-0.117626285855324,7.11112359239024E-5,
0.582563288526383));
#18321=CARTESIAN_POINT('Ctrl Pts',(-0.117492102008102,-0.0242809575267813,
0.584203936737797));
#18322=CARTESIAN_POINT('Ctrl Pts',(-0.0982512120079041,-0.0881067492982899,
0.588490914828312));
#18323=CARTESIAN_POINT('Ctrl Pts',(0.00631176444456456,-0.139064040754811,
0.595424222797929));
#18324=CARTESIAN_POINT('Ctrl Pts',(0.120263693490807,-0.0701091280034811,
0.603363212435234));
#18325=CARTESIAN_POINT('Ctrl Pts',(0.124122453355413,0.0630258865426945,
0.611302202072541));
#18326=CARTESIAN_POINT('Ctrl Pts',(0.0143556138404206,0.138465021405133,
0.619241191709845));
#18327=CARTESIAN_POINT('Ctrl Pts',(-0.0953630726970595,0.0926558297308384,
0.626328220527794));
#18328=CARTESIAN_POINT('Ctrl Pts',(-0.117475314221613,0.0265106736450616,
0.630768919466639));
#18329=CARTESIAN_POINT('Ctrl Pts',(-0.117676160015555,-9.46906955630045E-5,
0.632563288526383));
#18330=CARTESIAN_POINT('Ctrl Pts',(-0.11766919235599,-9.26074537421669E-5,
0.592436711473616));
#18331=CARTESIAN_POINT('Ctrl Pts',(-0.117764072896019,-0.0130062487266101,
0.593307528153066));
#18332=CARTESIAN_POINT('Ctrl Pts',(-0.109848366281979,-0.0650658641993071,
0.596825734206776));
#18333=CARTESIAN_POINT('Ctrl Pts',(-0.0336977294021144,-0.135086418755761,
0.602991329634746));
#18334=CARTESIAN_POINT('Ctrl Pts',(0.0952657566843092,-0.101529863106778,
0.610933497757526));
#18335=CARTESIAN_POINT('Ctrl Pts',(0.136956022624868,0.025038477707157,
0.618875665880307));
#18336=CARTESIAN_POINT('Ctrl Pts',(0.0531805018142573,0.128669000640787,
0.626817834003085));
#18337=CARTESIAN_POINT('Ctrl Pts',(-0.0778376600742765,0.114584191752874,
0.634671515867523));
#18338=CARTESIAN_POINT('Ctrl Pts',(-0.117856827377429,0.0376798124439797,
0.639877808357699));
#18339=CARTESIAN_POINT('Ctrl Pts',(-0.117962383120995,-2.41598447144253E-5,
0.642436711473616));
#18340=CARTESIAN_POINT('Origin',(0.,0.,-0.0924367114736175));
#18341=CARTESIAN_POINT('',(-0.117934829819181,5.63106208242181E-5,0.532563288526383));
#18342=CARTESIAN_POINT('',(-0.117629301205424,7.34277634442948E-5,0.542436711473615));
#18343=CARTESIAN_POINT('',(-0.117775,2.85464118895969E-14,-0.0924367114736175));
#18344=CARTESIAN_POINT('Ctrl Pts',(-0.117934829819181,5.63106208242166E-5,
0.532563288526383));
#18345=CARTESIAN_POINT('Ctrl Pts',(-0.117723349859012,-0.0357608023914865,
0.534992624129852));
#18346=CARTESIAN_POINT('Ctrl Pts',(-0.0811985738067347,-0.110967619805887,
0.540068289612422));
#18347=CARTESIAN_POINT('Ctrl Pts',(0.0467759446245483,-0.131113145053959,
0.547790284974095));
#18348=CARTESIAN_POINT('Ctrl Pts',(0.135526478334676,-0.031799677225719,
0.555729274611401));
#18349=CARTESIAN_POINT('Ctrl Pts',(0.100211809365564,0.0966242157284558,
0.563668264248707));
#18350=CARTESIAN_POINT('Ctrl Pts',(-0.0268399031138932,0.136595261273209,
0.571607253886012));
#18351=CARTESIAN_POINT('Ctrl Pts',(-0.108142973925314,0.0691035501437442,
0.577905595311905));
#18352=CARTESIAN_POINT('Ctrl Pts',(-0.117708537635025,0.0149983997031143,
0.581557606858695));
#18353=CARTESIAN_POINT('Ctrl Pts',(-0.117626285855324,7.11112359239024E-5,
0.582563288526383));
#18354=CARTESIAN_POINT('Ctrl Pts',(-0.117629301205424,7.34277634442983E-5,
0.542436711473615));
#18355=CARTESIAN_POINT('Ctrl Pts',(-0.11748956090956,-0.0244625652698295,
0.544089858574172));
#18356=CARTESIAN_POINT('Ctrl Pts',(-0.0980201725405651,-0.0884941619373469,
0.548390395048989));
#18357=CARTESIAN_POINT('Ctrl Pts',(0.00702343738442799,-0.139048728244533,
0.555338320898066));
#18358=CARTESIAN_POINT('Ctrl Pts',(0.12066450826877,-0.0694546898587181,
0.563280489020846));
#18359=CARTESIAN_POINT('Ctrl Pts',(0.123764493242992,0.063766979789076,
0.571222657143626));
#18360=CARTESIAN_POINT('Ctrl Pts',(0.0134834875971477,0.13857154491934,
0.579164825266405));
#18361=CARTESIAN_POINT('Ctrl Pts',(-0.0957036897026042,0.092147346049863,
0.586236176709736));
#18362=CARTESIAN_POINT('Ctrl Pts',(-0.117475624432153,0.0262528025703711,
0.590660138778806));
#18363=CARTESIAN_POINT('Ctrl Pts',(-0.11766919235599,-9.26074537421669E-5,
0.592436711473616));
#18364=CARTESIAN_POINT('Origin',(0.,0.,-0.0924367114736175));
#18365=CARTESIAN_POINT('',(-0.117794891956694,-0.000106411733115368,0.482563288526384));
#18366=CARTESIAN_POINT('',(-0.117936566864074,5.52347650140707E-5,0.492436711473616));
#18367=CARTESIAN_POINT('',(-0.117775,2.85464118895969E-14,-0.0924367114736175));
#18368=CARTESIAN_POINT('Ctrl Pts',(-0.117794891956694,-0.000106411733115381,
0.482563288526384));
#18369=CARTESIAN_POINT('Ctrl Pts',(-0.117872998614688,-0.00856127641466401,
0.483134981642805));
#18370=CARTESIAN_POINT('Ctrl Pts',(-0.113184542395844,-0.0560672187853419,
0.486353004638329));
#18371=CARTESIAN_POINT('Ctrl Pts',(-0.0487302328423073,-0.130399425645183,
0.492217357512954));
#18372=CARTESIAN_POINT('Ctrl Pts',(0.0831353173341669,-0.111656458896056,
0.50015634715026));
#18373=CARTESIAN_POINT('Ctrl Pts',(0.13889618212661,0.00930034365552528,
0.508095336787567));
#18374=CARTESIAN_POINT('Ctrl Pts',(0.0675071113591811,0.12174331898465,
0.516034326424871));
#18375=CARTESIAN_POINT('Ctrl Pts',(-0.0656800932930844,0.122738629397884,
0.523973316062178));
#18376=CARTESIAN_POINT('Ctrl Pts',(-0.116384786286051,0.04545243224792,
0.529482970096015));
#18377=CARTESIAN_POINT('Ctrl Pts',(-0.117953719733239,0.00325558390455253,
0.53234629425075));
#18378=CARTESIAN_POINT('Ctrl Pts',(-0.117934829819181,5.63106208242166E-5,
0.532563288526383));
#18379=CARTESIAN_POINT('Ctrl Pts',(-0.117936566864074,5.52347650140663E-5,
0.492436711473616));
#18380=CARTESIAN_POINT('Ctrl Pts',(-0.117728017843002,-0.0358510361847084,
0.494872188995279));
#18381=CARTESIAN_POINT('Ctrl Pts',(-0.0810366231971402,-0.111156550628637,
0.499955055891203));
#18382=CARTESIAN_POINT('Ctrl Pts',(0.0471380885036503,-0.131003351527116,
0.507685312161385));
#18383=CARTESIAN_POINT('Ctrl Pts',(0.135643160584381,-0.031381690295376,
0.515627480284167));
#18384=CARTESIAN_POINT('Ctrl Pts',(0.0998851624184703,0.0969888232104648,
0.523569648406945));
#18385=CARTESIAN_POINT('Ctrl Pts',(-0.0273779061153799,0.136507610615132,
0.531511816529727));
#18386=CARTESIAN_POINT('Ctrl Pts',(-0.108290992649607,0.0687756007668377,
0.537800837551949));
#18387=CARTESIAN_POINT('Ctrl Pts',(-0.117713344367368,0.0148299618267192,
0.541442469199912));
#18388=CARTESIAN_POINT('Ctrl Pts',(-0.117629301205424,7.34277634442983E-5,
0.542436711473615));
#18389=CARTESIAN_POINT('Origin',(0.,0.,-0.0924367114736175));
#18390=CARTESIAN_POINT('',(-0.117582256074849,9.06819982020624E-6,0.432563288526383));
#18391=CARTESIAN_POINT('',(-0.11779560903417,-0.000106574656651148,0.442436711473616));
#18392=CARTESIAN_POINT('',(-0.117775,2.85464118895969E-14,-0.0924367114736175));
#18393=CARTESIAN_POINT('Ctrl Pts',(-0.117582256074849,9.06819982019261E-6,
0.432563288526383));
#18394=CARTESIAN_POINT('Ctrl Pts',(-0.117568373935691,-0.020201912089319,
0.43392366903486));
#18395=CARTESIAN_POINT('Ctrl Pts',(-0.10300922874285,-0.0797477867736473,
0.437930379422439));
#18396=CARTESIAN_POINT('Ctrl Pts',(-0.00838939967687663,-0.138954178686792,
0.44458341968912));
#18397=CARTESIAN_POINT('Ctrl Pts',(0.11219917790857,-0.0824013973067221,
0.452522409326426));
#18398=CARTESIAN_POINT('Ctrl Pts',(0.13007709763057,0.0495842159710775,
0.460461398963732));
#18399=CARTESIAN_POINT('Ctrl Pts',(0.0288783492374893,0.136178877755608,
0.468400388601037));
#18400=CARTESIAN_POINT('Ctrl Pts',(-0.0895654556576369,0.100852400902523,
0.475767685121922));
#18401=CARTESIAN_POINT('Ctrl Pts',(-0.117511448025972,0.0305757367622385,
0.480488651763704));
#18402=CARTESIAN_POINT('Ctrl Pts',(-0.117794891956694,-0.000106411733115381,
0.482563288526384));
#18403=CARTESIAN_POINT('Ctrl Pts',(-0.11779560903417,-0.000106574656651151,
0.442436711473616));
#18404=CARTESIAN_POINT('Ctrl Pts',(-0.117873644338608,-0.00854245500997505,
0.443007130042126));
#18405=CARTESIAN_POINT('Ctrl Pts',(-0.113196618671047,-0.056044542179559,
0.446224937984896));
#18406=CARTESIAN_POINT('Ctrl Pts',(-0.0487473834415776,-0.130413074907061,
0.452090135301926));
#18407=CARTESIAN_POINT('Ctrl Pts',(0.0831820848081396,-0.111645054821459,
0.460032303424706));
#18408=CARTESIAN_POINT('Ctrl Pts',(0.138908217753341,0.00940130521287039,
0.467974471547486));
#18409=CARTESIAN_POINT('Ctrl Pts',(0.0673801526530663,0.121835103839429,
0.475916639670265));
#18410=CARTESIAN_POINT('Ctrl Pts',(-0.0658750545035054,0.12265543075329,
0.483858807793047));
#18411=CARTESIAN_POINT('Ctrl Pts',(-0.116424939330292,0.0453161125527027,
0.489365498394162));
#18412=CARTESIAN_POINT('Ctrl Pts',(-0.11795471279604,0.00317945345687678,
0.492224799621019));
#18413=CARTESIAN_POINT('Ctrl Pts',(-0.117936566864074,5.52347650140663E-5,
0.492436711473616));
#18414=CARTESIAN_POINT('Origin',(0.,0.,-0.0924367114736175));
#18415=CARTESIAN_POINT('',(-0.117828183671793,0.000101754196006455,0.382563288526383));
#18416=CARTESIAN_POINT('',(-0.117581664177921,7.09484545444172E-6,0.392436711473616));
#18417=CARTESIAN_POINT('',(-0.117775,2.85464118895969E-14,-0.0924367114736175));
#18418=CARTESIAN_POINT('Ctrl Pts',(-0.117828183671793,0.000101754196006446,
0.382563288526384));
#18419=CARTESIAN_POINT('Ctrl Pts',(-0.117538790254565,-0.0316580736410773,
0.384712356426916));
#18420=CARTESIAN_POINT('Ctrl Pts',(-0.0879068326507716,-0.103002379129266,
0.38950775420655));
#18421=CARTESIAN_POINT('Ctrl Pts',(0.0326876424682324,-0.135315053971568,
0.396949481865287));
#18422=CARTESIAN_POINT('Ctrl Pts',(0.13141703692502,-0.0459152284901983,
0.404888471502591));
#18423=CARTESIAN_POINT('Ctrl Pts',(0.109843140674695,0.0855168418978295,
0.412827461139898));
#18424=CARTESIAN_POINT('Ctrl Pts',(-0.0122846228212416,0.13866410438033,
0.420766450777203));
#18425=CARTESIAN_POINT('Ctrl Pts',(-0.104166535924894,0.0775181589932739,
0.427345059906032));
#18426=CARTESIAN_POINT('Ctrl Pts',(-0.117595378674006,0.0191142356295008,
0.431277339155758));
#18427=CARTESIAN_POINT('Ctrl Pts',(-0.117582256074849,9.06819982019261E-6,
0.432563288526383));
#18428=CARTESIAN_POINT('Ctrl Pts',(-0.117581664177921,7.09484545444172E-6,
0.392436711473616));
#18429=CARTESIAN_POINT('Ctrl Pts',(-0.117570873504463,-0.0200907396801347,
0.393789460463232));
#18430=CARTESIAN_POINT('Ctrl Pts',(-0.10312708440739,-0.079535468422451,
0.397789598827109));
#18431=CARTESIAN_POINT('Ctrl Pts',(-0.00873482453528946,-0.138951719454826,
0.404437126565246));
#18432=CARTESIAN_POINT('Ctrl Pts',(0.112042812448737,-0.0826455423945668,
0.412379294688026));
#18433=CARTESIAN_POINT('Ctrl Pts',(0.130177722634257,0.049372441998279,
0.420321462810806));
#18434=CARTESIAN_POINT('Ctrl Pts',(0.0290564652212241,0.136160197297018,
0.428263630933586));
#18435=CARTESIAN_POINT('Ctrl Pts',(-0.0895090212855029,0.100936776489487,
0.435635380487856));
#18436=CARTESIAN_POINT('Ctrl Pts',(-0.117511471984497,0.0306096014671689,
0.440359740667866));
#18437=CARTESIAN_POINT('Ctrl Pts',(-0.11779560903417,-0.000106574656651151,
0.442436711473616));
#18438=CARTESIAN_POINT('Origin',(0.,0.,-0.0924367114736175));
#18439=CARTESIAN_POINT('',(-0.117911328466355,-7.22474488887591E-5,0.332563288526384));
#18440=CARTESIAN_POINT('',(-0.117821685414254,0.000103165543095151,0.342436711473616));
#18441=CARTESIAN_POINT('',(-0.117775,2.85464118895969E-14,-0.0924367114736175));
#18442=CARTESIAN_POINT('Ctrl Pts',(-0.117911328466355,-7.22474488887752E-5,
0.332563288526384));
#18443=CARTESIAN_POINT('Ctrl Pts',(-0.117942332027964,-0.00437115939612809,
0.332854713939869));
#18444=CARTESIAN_POINT('Ctrl Pts',(-0.115777752883067,-0.0476754067323583,
0.335792469232457));
#18445=CARTESIAN_POINT('Ctrl Pts',(-0.0622106591311991,-0.12453304658572,
0.341376554404146));
#18446=CARTESIAN_POINT('Ctrl Pts',(0.0708961914151981,-0.119801401679107,
0.349315544041452));
#18447=CARTESIAN_POINT('Ctrl Pts',(0.1391024375543,-0.00539978406154301,
0.357254533678757));
#18448=CARTESIAN_POINT('Ctrl Pts',(0.0799699354250877,0.113944965792994,
0.365193523316063));
#18449=CARTESIAN_POINT('Ctrl Pts',(-0.0523695618881846,0.128980908622551,
0.373132512953369));
#18450=CARTESIAN_POINT('Ctrl Pts',(-0.113921748517257,0.0538356345748906,
0.378922434690143));
#18451=CARTESIAN_POINT('Ctrl Pts',(-0.117895144954496,0.00745050051778832,
0.382066026547814));
#18452=CARTESIAN_POINT('Ctrl Pts',(-0.117828183671793,0.000101754196006446,
0.382563288526384));
#18453=CARTESIAN_POINT('Ctrl Pts',(-0.117821685414254,0.000103165543095145,
0.342436711473616));
#18454=CARTESIAN_POINT('Ctrl Pts',(-0.117532262555972,-0.0314544122979593,
0.344571790884339));
#18455=CARTESIAN_POINT('Ctrl Pts',(-0.0882170202347594,-0.102616110661261,
0.349354259669323));
#18456=CARTESIAN_POINT('Ctrl Pts',(0.0320320385160992,-0.135491055083419,
0.356784117828566));
#18457=CARTESIAN_POINT('Ctrl Pts',(0.131227975626944,-0.0465090949381858,
0.364726285951346));
#18458=CARTESIAN_POINT('Ctrl Pts',(0.110205605501345,0.0850799742312894,
0.372668454074126));
#18459=CARTESIAN_POINT('Ctrl Pts',(-0.0117764211155082,0.138727046407055,
0.380610622196906));
#18460=CARTESIAN_POINT('Ctrl Pts',(-0.10403099481448,0.0777947493501838,
0.387200041330069));
#18461=CARTESIAN_POINT('Ctrl Pts',(-0.117591991327853,0.019241607989002,
0.391142071088973));
#18462=CARTESIAN_POINT('Ctrl Pts',(-0.117581664177921,7.09484545444172E-6,
0.392436711473616));
#18463=CARTESIAN_POINT('Origin',(0.,0.,-0.0924367114736175));
#18464=CARTESIAN_POINT('',(-0.117608153246896,-5.64262068778628E-5,0.282563288526383));
#18465=CARTESIAN_POINT('',(-0.117918861549493,-6.80329776671096E-5,0.292436711473615));
#18466=CARTESIAN_POINT('',(-0.117775,2.85464118895969E-14,-0.0924367114736175));
#18467=CARTESIAN_POINT('Ctrl Pts',(-0.117608153246896,-5.64262068778604E-5,
0.282563288526383));
#18468=CARTESIAN_POINT('Ctrl Pts',(-0.117677606263852,-0.0160946837114709,
0.283643401331924));
#18469=CARTESIAN_POINT('Ctrl Pts',(-0.107144424846824,-0.0713401098021974,
0.287369844016567));
#18470=CARTESIAN_POINT('Ctrl Pts',(-0.0229969941138309,-0.137294515779738,
0.293742616580312));
#18471=CARTESIAN_POINT('Ctrl Pts',(0.102883268653204,-0.0937746172089793,
0.301681606217617));
#18472=CARTESIAN_POINT('Ctrl Pts',(0.134580950019115,0.0355895166223291,
0.309620595854923));
#18473=CARTESIAN_POINT('Ctrl Pts',(0.0430789950773988,0.13237388709478,
0.317559585492229));
#18474=CARTESIAN_POINT('Ctrl Pts',(-0.0830523456774332,0.10887452531409,
0.325207149716049));
#18475=CARTESIAN_POINT('Ctrl Pts',(-0.11766079978112,0.0346657214219864,
0.330208384060767));
#18476=CARTESIAN_POINT('Ctrl Pts',(-0.117911328466355,-7.22474488887752E-5,
0.332563288526384));
#18477=CARTESIAN_POINT('Ctrl Pts',(-0.117918861549493,-6.80329776671157E-5,
0.292436711473616));
#18478=CARTESIAN_POINT('Ctrl Pts',(-0.117946256357307,-0.00405052459867665,
0.292706731931186));
#18479=CARTESIAN_POINT('Ctrl Pts',(-0.11595553950755,-0.0470512577090033,
0.295624141763016));
#18480=CARTESIAN_POINT('Ctrl Pts',(-0.0631725212350128,-0.124068972994571,
0.301188940969106));
#18481=CARTESIAN_POINT('Ctrl Pts',(0.0700327441786229,-0.12032993078169,
0.309131109091886));
#18482=CARTESIAN_POINT('Ctrl Pts',(0.139080821187468,-0.00635631000930847,
0.317073277214666));
#18483=CARTESIAN_POINT('Ctrl Pts',(0.0807165776729536,0.11344034374014,
0.325015445337446));
#18484=CARTESIAN_POINT('Ctrl Pts',(-0.0515923433190751,0.129313988454311,
0.332957613460226));
#18485=CARTESIAN_POINT('Ctrl Pts',(-0.113774867115171,0.0543021652640841,
0.338764702172283));
#18486=CARTESIAN_POINT('Ctrl Pts',(-0.117891132111753,0.00767537174388221,
0.341924401510079));
#18487=CARTESIAN_POINT('Ctrl Pts',(-0.117821685414254,0.000103165543095145,
0.342436711473616));
#18488=CARTESIAN_POINT('Origin',(0.,0.,-0.0924367114736175));
#18489=CARTESIAN_POINT('',(-0.117705188630573,0.000102098618198066,0.232563288526383));
#18490=CARTESIAN_POINT('',(-0.1176142238744,-6.23262858038681E-5,0.242436711473616));
#18491=CARTESIAN_POINT('',(-0.117775,2.85464118895969E-14,-0.0924367114736175));
#18492=CARTESIAN_POINT('Ctrl Pts',(-0.117705188630573,0.000102098618198071,
0.232563288526383));
#18493=CARTESIAN_POINT('Ctrl Pts',(-0.117475649963863,-0.0275896003179174,
0.234432088723979));
#18494=CARTESIAN_POINT('Ctrl Pts',(-0.0938913217252411,-0.0948462909608301,
0.238947218800678));
#18495=CARTESIAN_POINT('Ctrl Pts',(0.0182347644767634,-0.138007750384372,
0.246108678756477));
#18496=CARTESIAN_POINT('Ctrl Pts',(0.125841858853055,-0.0595186723796334,
0.254047668393783));
#18497=CARTESIAN_POINT('Ctrl Pts',(0.118249355954961,0.073455671106145,
0.261986658031089));
#18498=CARTESIAN_POINT('Ctrl Pts',(0.00240767183786234,0.139186381940956,
0.269925647668394));
#18499=CARTESIAN_POINT('Ctrl Pts',(-0.0995777503027144,0.0858938305448248,
0.27678452450016));
#18500=CARTESIAN_POINT('Ctrl Pts',(-0.117507442931816,0.0231998416616275,
0.280997071452822));
#18501=CARTESIAN_POINT('Ctrl Pts',(-0.117608153246896,-5.64262068778604E-5,
0.282563288526383));
#18502=CARTESIAN_POINT('Ctrl Pts',(-0.1176142238744,-6.2326285803882E-5,
0.242436711473616));
#18503=CARTESIAN_POINT('Ctrl Pts',(-0.117689148257971,-0.0156863246439697,
0.243489062352292));
#18504=CARTESIAN_POINT('Ctrl Pts',(-0.107519643382358,-0.0705218816827611,
0.247188802605229));
#18505=CARTESIAN_POINT('Ctrl Pts',(-0.024381182195918,-0.137074561658528,
0.253535932232426));
#18506=CARTESIAN_POINT('Ctrl Pts',(0.101985705091022,-0.094777599970642,
0.261478100355206));
#18507=CARTESIAN_POINT('Ctrl Pts',(0.134923209124943,0.0343453801629359,
0.269420268477986));
#18508=CARTESIAN_POINT('Ctrl Pts',(0.0442571924125319,0.132004463632409,
0.277362436600766));
#18509=CARTESIAN_POINT('Ctrl Pts',(-0.0824920331482911,0.109525057495754,
0.285034584265976));
#18510=CARTESIAN_POINT('Ctrl Pts',(-0.117677666622401,0.0349954280503056,
0.290059342556926));
#18511=CARTESIAN_POINT('Ctrl Pts',(-0.117918861549493,-6.80329776671157E-5,
0.292436711473616));
#18512=CARTESIAN_POINT('Origin',(0.,0.,-0.0924367114736175));
#18513=CARTESIAN_POINT('',(-0.117967994073432,-3.0724305424694E-6,0.182563288526383));
#18514=CARTESIAN_POINT('',(-0.117691121003631,9.91971943564221E-5,0.192436711473615));
#18515=CARTESIAN_POINT('',(-0.117775,2.85464118895969E-14,-0.0924367114736175));
#18516=CARTESIAN_POINT('Ctrl Pts',(-0.117967994073432,-3.07243054247449E-6,
0.182563288526383));
#18517=CARTESIAN_POINT('Ctrl Pts',(-0.117968057042159,-0.000167453844217198,
0.182574446236933));
#18518=CARTESIAN_POINT('Ctrl Pts',(-0.117893299674953,-0.0393189363008842,
0.185231933826584));
#18519=CARTESIAN_POINT('Ctrl Pts',(-0.0749972298318695,-0.11727771015962,
0.190535751295337));
#18520=CARTESIAN_POINT('Ctrl Pts',(0.0578663373665801,-0.126610160769685,
0.198474740932643));
#18521=CARTESIAN_POINT('Ctrl Pts',(0.13775723856723,-0.0200396862227523,
0.206413730569949));
#18522=CARTESIAN_POINT('Ctrl Pts',(0.091540828968026,0.104875747581476,
0.214352720207254));
#18523=CARTESIAN_POINT('Ctrl Pts',(-0.0384749358425138,0.133784622116252,
0.22229170984456));
#18524=CARTESIAN_POINT('Ctrl Pts',(-0.110955338697302,0.0622468391270206,
0.22836189928427));
#18525=CARTESIAN_POINT('Ctrl Pts',(-0.11780069007939,0.0116234575531164,
0.231785758844877));
#18526=CARTESIAN_POINT('Ctrl Pts',(-0.117705188630573,0.000102098618198071,
0.232563288526383));
#18527=CARTESIAN_POINT('Ctrl Pts',(-0.117691121003631,9.91971943564221E-5,
0.192436711473615));
#18528=CARTESIAN_POINT('Ctrl Pts',(-0.117474218986382,-0.0270951350261672,
0.194271392773399));
#18529=CARTESIAN_POINT('Ctrl Pts',(-0.0945676524372527,-0.0938598508209937,
0.198753463447442));
#18530=CARTESIAN_POINT('Ctrl Pts',(0.0165156171993534,-0.138242945169174,
0.205882923495746));
#18531=CARTESIAN_POINT('Ctrl Pts',(0.125131592687617,-0.061040658666823,
0.213825091618526));
#18532=CARTESIAN_POINT('Ctrl Pts',(0.119114174013628,0.0720811421096423,
0.221767259741306));
#18533=CARTESIAN_POINT('Ctrl Pts',(0.0039759348809324,0.139169211541763,
0.229709427864086));
#18534=CARTESIAN_POINT('Ctrl Pts',(-0.0990660356104632,0.0867677816679632,
0.236599245108189));
#18535=CARTESIAN_POINT('Ctrl Pts',(-0.117500661679058,0.0236188235484957,
0.240841672978032));
#18536=CARTESIAN_POINT('Ctrl Pts',(-0.1176142238744,-6.2326285803882E-5,
0.242436711473616));
#18537=CARTESIAN_POINT('Origin',(0.,0.,-0.0924367114736175));
#18538=CARTESIAN_POINT('',(-0.117696212882312,-0.000100181105204699,0.132563288526383));
#18539=CARTESIAN_POINT('',(-0.117967699956222,8.3697257429456E-6,0.142436711473616));
#18540=CARTESIAN_POINT('',(-0.117775,2.85464118895969E-14,-0.0924367114736175));
#18541=CARTESIAN_POINT('Ctrl Pts',(-0.117696212882312,-0.000100181105204706,
0.132563288526383));
#18542=CARTESIAN_POINT('Ctrl Pts',(-0.117792074781153,-0.0119544960022407,
0.133363133628988));
#18543=CARTESIAN_POINT('Ctrl Pts',(-0.110696412003459,-0.0629173266909915,
0.136809308610694));
#18544=CARTESIAN_POINT('Ctrl Pts',(-0.0373480950846616,-0.134103559412242,
0.142901813471503));
#18545=CARTESIAN_POINT('Ctrl Pts',(0.0924198687735613,-0.104101940294199,
0.150840803108809));
#18546=CARTESIAN_POINT('Ctrl Pts',(0.137583777756591,0.0211978768359354,
0.158779792746114));
#18547=CARTESIAN_POINT('Ctrl Pts',(0.0567991668878991,0.127092487218924,
0.16671878238342));
#18548=CARTESIAN_POINT('Ctrl Pts',(-0.0757945745091616,0.116657324056303,
0.174646614310176));
#18549=CARTESIAN_POINT('Ctrl Pts',(-0.117953122434976,0.0388197061692436,
0.179928116357831));
#18550=CARTESIAN_POINT('Ctrl Pts',(-0.117967994073432,-3.07243054247449E-6,
0.182563288526383));
#18551=CARTESIAN_POINT('Ctrl Pts',(-0.117967699956222,8.3697257429579E-6,
0.142436711473616));
#18552=CARTESIAN_POINT('Ctrl Pts',(-0.117928252023989,-0.038547130539091,
0.145053723194506));
#18553=CARTESIAN_POINT('Ctrl Pts',(-0.0762804946418446,-0.116178754198862,
0.150318124289656));
#18554=CARTESIAN_POINT('Ctrl Pts',(0.0559861945572589,-0.127473226882309,
0.158229914759066));
#18555=CARTESIAN_POINT('Ctrl Pts',(0.137471621702818,-0.0220324926503626,
0.166172082881846));
#18556=CARTESIAN_POINT('Ctrl Pts',(0.0930189202108026,0.103592267873211,
0.174114251004626));
#18557=CARTESIAN_POINT('Ctrl Pts',(-0.0366486683060043,0.134315868829211,
0.182056419127406));
#18558=CARTESIAN_POINT('Ctrl Pts',(-0.110544190454925,0.0633195416932908,
0.188163905950403));
#18559=CARTESIAN_POINT('Ctrl Pts',(-0.11778720200735,0.0121454601492482,
0.191624003399139));
#18560=CARTESIAN_POINT('Ctrl Pts',(-0.117691121003631,9.91971943564221E-5,
0.192436711473615));
#18561=CARTESIAN_POINT('Origin',(0.,0.,-0.0924367114736175));
#18562=CARTESIAN_POINT('',(-0.117613109409711,6.11591708146705E-5,0.0825632885263832));
#18563=CARTESIAN_POINT('',(-0.117715749944134,-0.000104199409386274,0.0924367114736155));
#18564=CARTESIAN_POINT('',(-0.117775,2.85464118895969E-14,-0.0924367114736175));
#18565=CARTESIAN_POINT('Ctrl Pts',(-0.117613109409711,6.11591708146765E-5,
0.0825632885263832));
#18566=CARTESIAN_POINT('Ctrl Pts',(-0.117502393620717,-0.0235240259785673,
0.0841518210210431));
#18567=CARTESIAN_POINT('Ctrl Pts',(-0.0991849320095013,-0.0865581493706475,
0.088386683394805));
#18568=CARTESIAN_POINT('Ctrl Pts',(0.00357853460314598,-0.139161043603659,
0.0952678756476685));
#18569=CARTESIAN_POINT('Ctrl Pts',(0.118863112008681,-0.0724583686054966,
0.103206865284975));
#18570=CARTESIAN_POINT('Ctrl Pts',(0.125336705278751,0.0605752693714656,
0.11114585492228));
#18571=CARTESIAN_POINT('Ctrl Pts',(0.0170731091066207,0.138156245709763,
0.119084844559586));
#18572=CARTESIAN_POINT('Ctrl Pts',(-0.094337657277608,0.0941904991302726,
0.126223989094287));
#18573=CARTESIAN_POINT('Ctrl Pts',(-0.11747491061231,0.0272661325996615,
0.130716803749886));
#18574=CARTESIAN_POINT('Ctrl Pts',(-0.117696212882312,-0.000100181105204706,
0.132563288526383));
#18575=CARTESIAN_POINT('Ctrl Pts',(-0.117715749944134,-0.000104199409386274,
0.0924367114736155));
#18576=CARTESIAN_POINT('Ctrl Pts',(-0.117810584636384,-0.011244028442556,
0.0931886642413524));
#18577=CARTESIAN_POINT('Ctrl Pts',(-0.111246641208053,-0.0614941526881817,
0.0965880063833492));
#18578=CARTESIAN_POINT('Ctrl Pts',(-0.0397151780004399,-0.133441281507892,
0.102634737899606));
#18579=CARTESIAN_POINT('Ctrl Pts',(0.0906220264938673,-0.105695447092796,
0.110576906022386));
#18580=CARTESIAN_POINT('Ctrl Pts',(0.137940159127448,0.0188783162799928,
0.118519074145166));
#18581=CARTESIAN_POINT('Ctrl Pts',(0.0588909273047484,0.126157580947307,
0.126461242267946));
#18582=CARTESIAN_POINT('Ctrl Pts',(-0.074108440039672,0.117863552156501,
0.134403410390726));
#18583=CARTESIAN_POINT('Ctrl Pts',(-0.117763087033452,0.0399060678969832,
0.139728566792616));
#18584=CARTESIAN_POINT('Ctrl Pts',(-0.117968157858494,0.000455912857932787,
0.142406333820246));
#18585=CARTESIAN_POINT('Ctrl Pts',(-0.117967699956222,8.3697257429579E-6,
0.142436711473616));
#18586=CARTESIAN_POINT('Origin',(0.,0.,-0.0924367114736175));
#18587=CARTESIAN_POINT('',(-0.117917485785546,7.60014832213593E-5,0.0325632885263832));
#18588=CARTESIAN_POINT('',(-0.117600989619072,5.04992496179954E-5,0.0424367114736154));
#18589=CARTESIAN_POINT('',(-0.117775,2.85464118895969E-14,-0.0924367114736175));
#18590=CARTESIAN_POINT('Ctrl Pts',(-0.117917485785546,7.60014832213644E-5,
0.0325632885263832));
#18591=CARTESIAN_POINT('Ctrl Pts',(-0.117676727567847,-0.0349830640657269,
0.0349405084130983));
#18592=CARTESIAN_POINT('Ctrl Pts',(-0.0825043195215805,-0.109517225708346,
0.0399640581789154));
#18593=CARTESIAN_POINT('Ctrl Pts',(0.0441923146003338,-0.131999388615902,
0.0476339378238343));
#18594=CARTESIAN_POINT('Ctrl Pts',(0.134874939024977,-0.034459980695041,
0.0555729274611401));
#18595=CARTESIAN_POINT('Ctrl Pts',(0.102091080224759,0.094638871230671,
0.0635119170984456));
#18596=CARTESIAN_POINT('Ctrl Pts',(-0.0241513666277066,0.137095110112719,
0.0714509067357516));
#18597=CARTESIAN_POINT('Ctrl Pts',(-0.107448046275642,0.0706698818446754,
0.0778013638783972));
#18598=CARTESIAN_POINT('Ctrl Pts',(-0.117686834607281,0.0157664388843013,
0.0815054911419412));
#18599=CARTESIAN_POINT('Ctrl Pts',(-0.117613109409711,6.11591708146765E-5,
0.0825632885263832));
#18600=CARTESIAN_POINT('Ctrl Pts',(-0.117600989619072,5.04992496179954E-5,
0.0424367114736154));
#18601=CARTESIAN_POINT('Ctrl Pts',(-0.117514779739531,-0.0227353060542692,
0.043970994662459));
#18602=CARTESIAN_POINT('Ctrl Pts',(-0.100129952091853,-0.0849605109884783,
0.0481526672255625));
#18603=CARTESIAN_POINT('Ctrl Pts',(0.000787973702835166,-0.139222729671589,
0.054981729162926));
#18604=CARTESIAN_POINT('Ctrl Pts',(0.117431922513572,-0.0747907597173192,
0.0629238972857061));
#18605=CARTESIAN_POINT('Ctrl Pts',(0.126496838785129,0.0581591461343325,
0.070866065408486));
#18606=CARTESIAN_POINT('Ctrl Pts',(0.0196773008918215,0.137828289815661,
0.0788082335312661));
#18607=CARTESIAN_POINT('Ctrl Pts',(-0.0933482651079043,0.0956446566614129,
0.085998448886309));
#18608=CARTESIAN_POINT('Ctrl Pts',(-0.11747670148927,0.0279758085988667,
0.0905412748670923));
#18609=CARTESIAN_POINT('Ctrl Pts',(-0.117715749944134,-0.000104199409386274,
0.0924367114736155));
#18610=CARTESIAN_POINT('Origin',(0.,0.,1.55));
#18611=CARTESIAN_POINT('',(-0.143211704627722,-5.70397197726547E-6,1.50700023576178));
#18612=CARTESIAN_POINT('Ctrl Pts',(-0.0334019664626774,0.112939183906323,
1.532225));
#18613=CARTESIAN_POINT('Ctrl Pts',(-0.0250606930336426,0.115799676338094,
1.53184761307169));
#18614=CARTESIAN_POINT('Ctrl Pts',(-0.0164287086124659,0.117635554524944,
1.53147359869818));
#18615=CARTESIAN_POINT('Ctrl Pts',(-0.00767226928320402,0.118510614220874,
1.53110056493424));
#18616=CARTESIAN_POINT('Ctrl Pts',(-0.0042150196872779,0.118856108509867,
1.53095328237096));
#18617=CARTESIAN_POINT('Ctrl Pts',(-0.000736351480830917,0.119051293525916,
1.53080607672538));
#18618=CARTESIAN_POINT('Ctrl Pts',(0.00274830211697625,0.119097943881266,
1.53065904037218));
#18619=CARTESIAN_POINT('Ctrl Pts',(0.00972321854123044,0.119191319684798,
1.53036473098213));
#18620=CARTESIAN_POINT('Ctrl Pts',(0.0166907125456733,0.118690968429664,
1.53007241075126));
#18621=CARTESIAN_POINT('Ctrl Pts',(0.0235721318645625,0.11762150546261,
1.52978094357425));
#18622=CARTESIAN_POINT('Ctrl Pts',(0.0273478463565568,0.117034709826966,
1.52962102062912));
#18623=CARTESIAN_POINT('Ctrl Pts',(0.0310977188904398,0.116276259986281,
1.52946135449799));
#18624=CARTESIAN_POINT('Ctrl Pts',(0.0348087249896146,0.115347945392283,
1.52930175751644));
#18625=CARTESIAN_POINT('Ctrl Pts',(0.0378768737129624,0.114580442682688,
1.52916980751093));
#18626=CARTESIAN_POINT('Ctrl Pts',(0.0409182562642153,0.113696477767379,
1.52903790896105));
#18627=CARTESIAN_POINT('Ctrl Pts',(0.0439120268522727,0.112701821307647,
1.52890655030309));
#18628=CARTESIAN_POINT('Ctrl Pts',(0.0504861734289241,0.110517613410832,
1.52861809430882));
#18629=CARTESIAN_POINT('Ctrl Pts',(0.0568477403450367,0.107796947733889,
1.528331525126));
#18630=CARTESIAN_POINT('Ctrl Pts',(0.0629211062797432,0.10455513280498,
1.52804576869741));
#18631=CARTESIAN_POINT('Ctrl Pts',(0.0667529140263229,0.102509807084265,
1.52786547926507));
#18632=CARTESIAN_POINT('Ctrl Pts',(0.0704699809867569,0.100256700264741,
1.52768551335768));
#18633=CARTESIAN_POINT('Ctrl Pts',(0.0740519796445933,0.0977963961590643,
1.52750560123222));
#18634=CARTESIAN_POINT('Ctrl Pts',(0.0761474027326905,0.0963571499395001,
1.52740035495562));
#18635=CARTESIAN_POINT('Ctrl Pts',(0.0781972522873126,0.0948464165467323,
1.52729509152825));
#18636=CARTESIAN_POINT('Ctrl Pts',(0.0801950758490376,0.0932655888959708,
1.52718986717129));
#18637=CARTESIAN_POINT('Ctrl Pts',(0.0872135629190184,0.0877120362002772,
1.52682020700562));
#18638=CARTESIAN_POINT('Ctrl Pts',(0.0935342345834078,0.0813437113039547,
1.52645409167081));
#18639=CARTESIAN_POINT('Ctrl Pts',(0.0991216768718319,0.0743433873765979,
1.52608928877518));
#18640=CARTESIAN_POINT('Ctrl Pts',(0.101857856375295,0.0709153174549959,
1.52591064420861));
#18641=CARTESIAN_POINT('Ctrl Pts',(0.104417791592617,0.0673349702414553,
1.52573231437502));
#18642=CARTESIAN_POINT('Ctrl Pts',(0.106794530290299,0.0636205708890664,
1.52555403711528));
#18643=CARTESIAN_POINT('Ctrl Pts',(0.108394385735532,0.0611202951812291,
1.52543403324399));
#18644=CARTESIAN_POINT('Ctrl Pts',(0.109912312880749,0.0585571637778213,
1.52531395827658));
#18645=CARTESIAN_POINT('Ctrl Pts',(0.111341951189028,0.0559432008961949,
1.5251940432238));
#18646=CARTESIAN_POINT('Ctrl Pts',(0.115894033640165,0.0476201345006791,
1.52481222412716));
#18647=CARTESIAN_POINT('Ctrl Pts',(0.119530893641226,0.0388304356906876,
1.52443409356659));
#18648=CARTESIAN_POINT('Ctrl Pts',(0.122195159250079,0.0297595052710396,
1.52405718851832));
#18649=CARTESIAN_POINT('Ctrl Pts',(0.123464283518865,0.0254385629829291,
1.52387764960816));
#18650=CARTESIAN_POINT('Ctrl Pts',(0.124512110981915,0.0210533134598664,
1.52369838877875));
#18651=CARTESIAN_POINT('Ctrl Pts',(0.12532867129748,0.0166220814218575,
1.52351913980531));
#18652=CARTESIAN_POINT('Ctrl Pts',(0.126067828800149,0.012610891624201,
1.52335688207487));
#18653=CARTESIAN_POINT('Ctrl Pts',(0.12661735951473,0.00855739899605222,
1.52319445303817));
#18654=CARTESIAN_POINT('Ctrl Pts',(0.126966826155483,0.00450415768051923,
1.52303280899981));
#18655=CARTESIAN_POINT('Ctrl Pts',(0.127602972227412,-0.00287409603749457,
1.52273856283131));
#18656=CARTESIAN_POINT('Ctrl Pts',(0.12758177643555,-0.010267620141741,
1.52244625042084));
#18657=CARTESIAN_POINT('Ctrl Pts',(0.126865581413421,-0.0175939782534482,
1.52215473434257));
#18658=CARTESIAN_POINT('Ctrl Pts',(0.126426462283551,-0.0220859726121444,
1.52197599770985));
#18659=CARTESIAN_POINT('Ctrl Pts',(0.12572570473317,-0.0265528301690258,
1.52179756043894));
#18660=CARTESIAN_POINT('Ctrl Pts',(0.124776542651163,-0.0309793260681717,
1.52161916036391));
#18661=CARTESIAN_POINT('Ctrl Pts',(0.124151644840291,-0.0338935887106027,
1.52150170748789));
#18662=CARTESIAN_POINT('Ctrl Pts',(0.123418330834614,-0.0367926408403149,
1.52138417707714));
#18663=CARTESIAN_POINT('Ctrl Pts',(0.122581975874549,-0.0396644408336013,
1.52126680258073));
#18664=CARTESIAN_POINT('Ctrl Pts',(0.120074191833131,-0.0482754427851461,
1.52091485884509));
#18665=CARTESIAN_POINT('Ctrl Pts',(0.116656903439717,-0.0566007293654626,
1.52056600333313));
#18666=CARTESIAN_POINT('Ctrl Pts',(0.112443760417108,-0.0645262187619275,
1.52021830866717));
#18667=CARTESIAN_POINT('Ctrl Pts',(0.109356904590302,-0.0703330102694749,
1.51996356219884));
#18668=CARTESIAN_POINT('Ctrl Pts',(0.105841781173658,-0.0759253337267248,
1.51970943888381));
#18669=CARTESIAN_POINT('Ctrl Pts',(0.101930367117466,-0.0812537151913617,
1.51945518067311));
#18670=CARTESIAN_POINT('Ctrl Pts',(0.100130771446666,-0.0837052409256295,
1.51933819945644));
#18671=CARTESIAN_POINT('Ctrl Pts',(0.0982476276828181,-0.0860996963839449,
1.51922123442864));
#18672=CARTESIAN_POINT('Ctrl Pts',(0.0962924325256194,-0.0884227179472683,
1.51910469697823));
#18673=CARTESIAN_POINT('Ctrl Pts',(0.0906946176521128,-0.0950736369671782,
1.51877104482549));
#18674=CARTESIAN_POINT('Ctrl Pts',(0.0844921899154374,-0.101162815315101,
1.51843983772287));
#18675=CARTESIAN_POINT('Ctrl Pts',(0.0777644521522082,-0.106582693579069,
1.51810941878));
#18676=CARTESIAN_POINT('Ctrl Pts',(0.0731067700043679,-0.110334931124879,
1.5178806663426));
#18677=CARTESIAN_POINT('Ctrl Pts',(0.0681966627772886,-0.113766151308436,
1.51765229166508));
#18678=CARTESIAN_POINT('Ctrl Pts',(0.0630541948599911,-0.116833686038022,
1.5174237449583));
#18679=CARTESIAN_POINT('Ctrl Pts',(0.0607686815400033,-0.118197018118406,
1.51732216988754));
#18680=CARTESIAN_POINT('Ctrl Pts',(0.0584414404741937,-0.119485783651375,
1.51722075040181));
#18681=CARTESIAN_POINT('Ctrl Pts',(0.0560784264268894,-0.12069488199044,
1.51711960151386));
#18682=CARTESIAN_POINT('Ctrl Pts',(0.0475595529450054,-0.125053787850271,
1.51675495087613));
#18683=CARTESIAN_POINT('Ctrl Pts',(0.038563113830939,-0.128389854466075,
1.51639315730301));
#18684=CARTESIAN_POINT('Ctrl Pts',(0.0292711048986314,-0.130741856378471,
1.51603205677802));
#18685=CARTESIAN_POINT('Ctrl Pts',(0.0254547302664753,-0.13170786066222,
1.51588374709674));
#18686=CARTESIAN_POINT('Ctrl Pts',(0.0215881861914954,-0.132507324978224,
1.51573555432397));
#18687=CARTESIAN_POINT('Ctrl Pts',(0.0176832233642019,-0.13314066674995,
1.51558732853105));
#18688=CARTESIAN_POINT('Ctrl Pts',(0.0144414794405867,-0.133666441752394,
1.51546427740745));
#18689=CARTESIAN_POINT('Ctrl Pts',(0.0111713231872828,-0.134077605234841,
1.5153411329761));
#18690=CARTESIAN_POINT('Ctrl Pts',(0.00789687394913892,-0.134372952697723,
1.51521845803943));
#18691=CARTESIAN_POINT('Ctrl Pts',(-0.00208492598009478,-0.135273287095873,
1.51484449692866));
#18692=CARTESIAN_POINT('Ctrl Pts',(-0.0121386692885745,-0.135107999768821,
1.51447364169918));
#18693=CARTESIAN_POINT('Ctrl Pts',(-0.0220717676774029,-0.133899092645375,
1.51410356562093));
#18694=CARTESIAN_POINT('Ctrl Pts',(-0.0271373055616968,-0.133282591671289,
1.51391483957382));
#18695=CARTESIAN_POINT('Ctrl Pts',(-0.0321716696217597,-0.132393849601707,
1.51372631615657));
#18696=CARTESIAN_POINT('Ctrl Pts',(-0.0371491047637803,-0.131230566976147,
1.51353768678866));
#18697=CARTESIAN_POINT('Ctrl Pts',(-0.0401763453142056,-0.130523066780721,
1.51342296375255));
#18698=CARTESIAN_POINT('Ctrl Pts',(-0.0431793745847511,-0.129714439573166,
1.51330831773957));
#18699=CARTESIAN_POINT('Ctrl Pts',(-0.0461427198170546,-0.128807808452418,
1.51319405707679));
#18700=CARTESIAN_POINT('Ctrl Pts',(-0.0557912886485991,-0.125855842991896,
1.51282202756853));
#18701=CARTESIAN_POINT('Ctrl Pts',(-0.0650506639775802,-0.121862017750276,
1.51245293010828));
#18702=CARTESIAN_POINT('Ctrl Pts',(-0.0737251756215706,-0.116823260910032,
1.51208446868514));
#18703=CARTESIAN_POINT('Ctrl Pts',(-0.0774533877539874,-0.114657657224767,
1.51192610791459));
#18704=CARTESIAN_POINT('Ctrl Pts',(-0.0810733781510443,-0.112298364258586,
1.51176786463208));
#18705=CARTESIAN_POINT('Ctrl Pts',(-0.0845783705992567,-0.109758519633299,
1.51160955655689));
#18706=CARTESIAN_POINT('Ctrl Pts',(-0.0871260289206952,-0.107912394030924,
1.51149448786814));
#18707=CARTESIAN_POINT('Ctrl Pts',(-0.0896122610481647,-0.105970921032248,
1.51137940572563));
#18708=CARTESIAN_POINT('Ctrl Pts',(-0.0920243025666997,-0.10394826075131,
1.51126473391974));
#18709=CARTESIAN_POINT('Ctrl Pts',(-0.0995315444015674,-0.0976529296958118,
1.51090782920982));
#18710=CARTESIAN_POINT('Ctrl Pts',(-0.106349817996106,-0.090554906599088,
1.51055366538392));
#18711=CARTESIAN_POINT('Ctrl Pts',(-0.112409916721278,-0.0828189535999138,
1.51020021897155));
#18712=CARTESIAN_POINT('Ctrl Pts',(-0.11567060314877,-0.0786565598680515,
1.51001004419521));
#18713=CARTESIAN_POINT('Ctrl Pts',(-0.118711357121208,-0.0743087544864998,
1.50982007711492));
#18714=CARTESIAN_POINT('Ctrl Pts',(-0.121517490738653,-0.0697974244982526,
1.50963000253165));
#18715=CARTESIAN_POINT('Ctrl Pts',(-0.123184827969132,-0.0671169005197731,
1.50951706477726));
#18716=CARTESIAN_POINT('Ctrl Pts',(-0.124768226583796,-0.064379797453554,
1.50940414472167));
#18717=CARTESIAN_POINT('Ctrl Pts',(-0.12625918933752,-0.0616017405091787,
1.50929161182319));
#18718=CARTESIAN_POINT('Ctrl Pts',(-0.131254477666307,-0.0522942005345653,
1.50891458411209));
#18719=CARTESIAN_POINT('Ctrl Pts',(-0.135235816373665,-0.0424980109473837,
1.50854057440173));
#18720=CARTESIAN_POINT('Ctrl Pts',(-0.138100316247284,-0.0323932585971084,
1.50816719719795));
#18721=CARTESIAN_POINT('Ctrl Pts',(-0.139428601593765,-0.027707625827389,
1.5079940600046));
#18722=CARTESIAN_POINT('Ctrl Pts',(-0.140516076092011,-0.0229552175461711,
1.50782105881478));
#18723=CARTESIAN_POINT('Ctrl Pts',(-0.14134846970832,-0.01815262603916,
1.50764795577689));
#18724=CARTESIAN_POINT('Ctrl Pts',(-0.141840021659925,-0.0153165600461233,
1.5075457335416));
#18725=CARTESIAN_POINT('Ctrl Pts',(-0.142241997144177,-0.0124651428186592,
1.50744355431084));
#18726=CARTESIAN_POINT('Ctrl Pts',(-0.142550993842162,-0.00961078035088443,
1.50734168592779));
#18727=CARTESIAN_POINT('Ctrl Pts',(-0.142847161918882,-0.00687492249914849,
1.50724404681617));
#18728=CARTESIAN_POINT('Ctrl Pts',(-0.143058332724879,-0.00413406598225375,
1.5071466105924));
#18729=CARTESIAN_POINT('Ctrl Pts',(-0.143182669649515,-0.00139134585336764,
1.50704933585643));
#18730=CARTESIAN_POINT('Ctrl Pts',(-0.143203595382121,-0.00092974984559876,
1.50703296465278));
#18731=CARTESIAN_POINT('Ctrl Pts',(-0.143222061023464,-0.000468100854706259,
1.50701659802318));
#18732=CARTESIAN_POINT('Ctrl Pts',(-0.143238079070951,-6.41379011939899E-6,
1.50700023577028));
#18733=CARTESIAN_POINT('',(-0.00156744678985144,0.146109855568756,1.50365));
#18734=CARTESIAN_POINT('Ctrl Pts',(-0.00156962371672063,0.146072546381438,
1.50365));
#18735=CARTESIAN_POINT('Ctrl Pts',(-0.011711474284147,0.144648739717271,
1.50495065132295));
#18736=CARTESIAN_POINT('Ctrl Pts',(-0.0216501921041044,0.142222471223284,
1.50626105010813));
#18737=CARTESIAN_POINT('Ctrl Pts',(-0.0312062965385204,0.138804788898175,
1.50759029209282));
#18738=CARTESIAN_POINT('Ctrl Pts',(-0.0379863325344082,0.136379950477271,
1.50853338648503));
#18739=CARTESIAN_POINT('Ctrl Pts',(-0.0445735484268955,0.133455002060128,
1.5094859663039));
#18740=CARTESIAN_POINT('Ctrl Pts',(-0.0508923708069948,0.130021662144985,
1.51045128011208));
#18741=CARTESIAN_POINT('Ctrl Pts',(-0.053607485163773,0.128546401418451,
1.51086606268101));
#18742=CARTESIAN_POINT('Ctrl Pts',(-0.0562647183424556,0.126981576978965,
1.51128195276517));
#18743=CARTESIAN_POINT('Ctrl Pts',(-0.0588579379029418,0.125328026221608,
1.51169910067666));
#18744=CARTESIAN_POINT('Ctrl Pts',(-0.0624505046767585,0.123037247762191,
1.51227700458785));
#18745=CARTESIAN_POINT('Ctrl Pts',(-0.0659209207101175,0.120575889029892,
1.51285741907924));
#18746=CARTESIAN_POINT('Ctrl Pts',(-0.0692542752175272,0.117943487410649,
1.51344114883776));
#18747=CARTESIAN_POINT('Ctrl Pts',(-0.0735613784355843,0.114542101371374,
1.51419539934302));
#18748=CARTESIAN_POINT('Ctrl Pts',(-0.0776398170223455,0.110855132244726,
1.51495518495604));
#18749=CARTESIAN_POINT('Ctrl Pts',(-0.0814741368103916,0.106911749311875,
1.51572224163114));
#18750=CARTESIAN_POINT('Ctrl Pts',(-0.0845038784997064,0.103795829845314,
1.51632834224744));
#18751=CARTESIAN_POINT('Ctrl Pts',(-0.087381117690253,0.10051973853988,
1.51693898261853));
#18752=CARTESIAN_POINT('Ctrl Pts',(-0.0900959757046659,0.0970973798321736,
1.51755501917095));
#18753=CARTESIAN_POINT('Ctrl Pts',(-0.0920052356275281,0.0946905606587243,
1.51798825505079));
#18754=CARTESIAN_POINT('Ctrl Pts',(-0.093830595110286,0.092215607777745,
1.51842338946406));
#18755=CARTESIAN_POINT('Ctrl Pts',(-0.0955653742165971,0.0896840982544811,
1.51885969689116));
#18756=CARTESIAN_POINT('Ctrl Pts',(-0.0997851775729162,0.0835262696618028,
1.51992100293214));
#18757=CARTESIAN_POINT('Ctrl Pts',(-0.103479134251024,0.0770231540939269,
1.52099120961793));
#18758=CARTESIAN_POINT('Ctrl Pts',(-0.106606394578922,0.0702509006766953,
1.52207541818308));
#18759=CARTESIAN_POINT('Ctrl Pts',(-0.108879606303698,0.0653281362576702,
1.52286353153598));
#18760=CARTESIAN_POINT('Ctrl Pts',(-0.110852991156964,0.0602629640702717,
1.52365904329275));
#18761=CARTESIAN_POINT('Ctrl Pts',(-0.112503888351057,0.0550849881514033,
1.524463912762));
#18762=CARTESIAN_POINT('Ctrl Pts',(-0.113450017754745,0.0521174894567802,
1.52492518356294));
#18763=CARTESIAN_POINT('Ctrl Pts',(-0.114289979676541,0.0491121240008169,
1.52538965304266));
#18764=CARTESIAN_POINT('Ctrl Pts',(-0.115015874151616,0.0460903162170444,
1.52585530945224));
#18765=CARTESIAN_POINT('Ctrl Pts',(-0.117053612444637,0.0376074669234184,
1.52716250482259));
#18766=CARTESIAN_POINT('Ctrl Pts',(-0.118206139871793,0.0289652499882669,
1.52848357355921));
#18767=CARTESIAN_POINT('Ctrl Pts',(-0.11838625730212,0.0202925750432425,
1.52982832573377));
#18768=CARTESIAN_POINT('Ctrl Pts',(-0.118492077855379,0.015197303257165,
1.53061837930521));
#18769=CARTESIAN_POINT('Ctrl Pts',(-0.118261361656021,0.0100916471271278,
1.53141660760476));
#18770=CARTESIAN_POINT('Ctrl Pts',(-0.11766859746431,0.00500517689818842,
1.532225));
#18771=CARTESIAN_POINT('',(-0.115079981391543,0.0902137050004572,1.50365));
#18772=CARTESIAN_POINT('Origin',(0.,0.,1.50365));
#18773=CARTESIAN_POINT('Ctrl Pts',(-0.143238079070951,-6.41379011939899E-6,
1.50700023577028));
#18774=CARTESIAN_POINT('Ctrl Pts',(-0.143514357617001,0.00795674345750163,
1.50671802038504));
#18775=CARTESIAN_POINT('Ctrl Pts',(-0.14306421847979,0.0159310909218757,
1.50643710681857));
#18776=CARTESIAN_POINT('Ctrl Pts',(-0.141940608246003,0.023841490005315,
1.50615648267927));
#18777=CARTESIAN_POINT('Ctrl Pts',(-0.141317731836386,0.0282266413964,1.50600091791928));
#18778=CARTESIAN_POINT('Ctrl Pts',(-0.14048752132733,0.0325921818867556,
1.50584544210227));
#18779=CARTESIAN_POINT('Ctrl Pts',(-0.139456452513291,0.0369250818702156,
1.5056898827608));
#18780=CARTESIAN_POINT('Ctrl Pts',(-0.138790989895207,0.0397215809279161,
1.50558948313156));
#18781=CARTESIAN_POINT('Ctrl Pts',(-0.138042009924554,0.0425029011667524,
1.50548910366784));
#18782=CARTESIAN_POINT('Ctrl Pts',(-0.137214434473447,0.0452564915355094,
1.50538902890071));
#18783=CARTESIAN_POINT('Ctrl Pts',(-0.134176751889031,0.0553637675507716,
1.50502169637912));
#18784=CARTESIAN_POINT('Ctrl Pts',(-0.130076454936343,0.0651325632434767,
1.50465723703036));
#18785=CARTESIAN_POINT('Ctrl Pts',(-0.125018127980614,0.0743940890034878,
1.50429344851366));
#18786=CARTESIAN_POINT('Ctrl Pts',(-0.122034683484208,0.0798566160996726,
1.50407888293545));
#18787=CARTESIAN_POINT('Ctrl Pts',(-0.118716925567465,0.0851425936725427,
1.50386455072235));
#18788=CARTESIAN_POINT('Ctrl Pts',(-0.115078604842436,0.0902138214954005,
1.50365));
#18789=CARTESIAN_POINT('',(-0.05,-6.12323399573677E-18,1.6));
#18790=CARTESIAN_POINT('',(-0.1,-1.22464679914735E-17,1.55));
#18791=CARTESIAN_POINT('Origin',(0.,0.,1.6));
#18792=CARTESIAN_POINT('Ctrl Pts',(0.0850780204044575,-0.11908002747757,
-0.0164977839420936));
#18793=CARTESIAN_POINT('Ctrl Pts',(0.124677800165771,-0.0907875342533835,
-0.0138514540629917));
#18794=CARTESIAN_POINT('Ctrl Pts',(0.172751483861701,0.00791416360185712,
-0.00855879430478784));
#18795=CARTESIAN_POINT('Ctrl Pts',(0.0868617128612901,0.149726167188418,
-0.000619804667482127));
#18796=CARTESIAN_POINT('Ctrl Pts',(-0.078614020905812,0.154028602276276,
0.00731918496982359));
#18797=CARTESIAN_POINT('Ctrl Pts',(-0.172087192378165,0.0175525219725009,
0.0152581746071293));
#18798=CARTESIAN_POINT('Ctrl Pts',(-0.108045720411827,-0.135108484733225,
0.0231971642444351));
#18799=CARTESIAN_POINT('Ctrl Pts',(0.0549144151285058,-0.164025561655164,
0.0311361538817407));
#18800=CARTESIAN_POINT('Ctrl Pts',(0.167598788591005,-0.0428207868793744,
0.0390751435190465));
#18801=CARTESIAN_POINT('Ctrl Pts',(0.126860790413016,0.117600499296196,
0.0470141331563521));
#18802=CARTESIAN_POINT('Ctrl Pts',(-0.0300110592737492,0.170357625684536,
0.054953122793658));
#18803=CARTESIAN_POINT('Ctrl Pts',(-0.159409054995301,0.0671687418111174,
0.0628921124309635));
#18804=CARTESIAN_POINT('Ctrl Pts',(-0.142879399887002,-0.0975110083167992,
0.0708311020682695));
#18805=CARTESIAN_POINT('Ctrl Pts',(0.00444677171871267,-0.172924803493063,
0.078770091705575));
#18806=CARTESIAN_POINT('Ctrl Pts',(0.147702113712341,-0.0900384822365835,
0.0867090813428809));
#18807=CARTESIAN_POINT('Ctrl Pts',(0.155746353789385,0.0752722621313087,
0.0946480709801864));
#18808=CARTESIAN_POINT('Ctrl Pts',(0.021215449100004,0.17167621786987,0.102587060617492));
#18809=CARTESIAN_POINT('Ctrl Pts',(-0.132736728465598,0.110922462699857,
0.110526050254798));
#18810=CARTESIAN_POINT('Ctrl Pts',(-0.165177537004225,-0.0513732581591355,
0.118465039892104));
#18811=CARTESIAN_POINT('Ctrl Pts',(-0.0464096261145344,-0.166640254043574,
0.126404029529409));
#18812=CARTESIAN_POINT('Ctrl Pts',(0.114843114370719,-0.129359532685675,
0.134343019166715));
#18813=CARTESIAN_POINT('Ctrl Pts',(0.170964855654229,0.0263409830179588,
0.142282008804021));
#18814=CARTESIAN_POINT('Ctrl Pts',(0.0705799878925336,0.157928129946847,
0.150220998441327));
#18815=CARTESIAN_POINT('Ctrl Pts',(-0.0944160212638482,0.144942899583874,
0.158159988078632));
#18816=CARTESIAN_POINT('Ctrl Pts',(-0.172980633894512,-0.000727622896455919,
0.166098977715938));
#18817=CARTESIAN_POINT('Ctrl Pts',(-0.0931933312323777,-0.145732055885043,
0.174037967353244));
#18818=CARTESIAN_POINT('Ctrl Pts',(0.0719060791645076,-0.157328779695546,
0.181976956990549));
#18819=CARTESIAN_POINT('Ctrl Pts',(0.171180402159323,-0.0249017879745179,
0.189915946627855));
#18820=CARTESIAN_POINT('Ctrl Pts',(0.113750798721884,0.13032108391891,0.197854936265161));
#18821=CARTESIAN_POINT('Ctrl Pts',(-0.0478098650864174,0.16624393501773,
0.205793925902467));
#18822=CARTESIAN_POINT('Ctrl Pts',(-0.16560387403618,0.0499818570245514,
0.213732915539772));
#18823=CARTESIAN_POINT('Ctrl Pts',(-0.131798885878402,-0.112035185581475,
0.221671905177078));
#18824=CARTESIAN_POINT('Ctrl Pts',(0.0226589495323734,-0.171491694067101,
0.229610894814384));
#18825=CARTESIAN_POINT('Ctrl Pts',(0.156374069566079,-0.073959309724122,
0.237549884451689));
#18826=CARTESIAN_POINT('Ctrl Pts',(0.146939445926624,0.0912777539068999,
0.245488874088995));
#18827=CARTESIAN_POINT('Ctrl Pts',(0.00299182995941577,0.172956289510158,
0.253427863726301));
#18828=CARTESIAN_POINT('Ctrl Pts',(-0.143694601292225,0.0963051955349955,
0.261366853363607));
#18829=CARTESIAN_POINT('Ctrl Pts',(-0.15883847309497,-0.0685067047260848,
0.269305843000912));
#18830=CARTESIAN_POINT('Ctrl Pts',(-0.0285766086907934,-0.170605411881679,
0.277244832638218));
#18831=CARTESIAN_POINT('Ctrl Pts',(0.12784518248692,-0.116526556812001,
0.285183822275524));
#18832=CARTESIAN_POINT('Ctrl Pts',(0.167233470900423,0.0442243749325307,
0.293122811912829));
#18833=CARTESIAN_POINT('Ctrl Pts',(0.0535309779628647,0.164490922320707,
0.301061801550136));
#18834=CARTESIAN_POINT('Ctrl Pts',(-0.109175456582181,0.134177303623408,
0.309000791187441));
#18835=CARTESIAN_POINT('Ctrl Pts',(-0.171939242908932,-0.0189664407699395,
0.316939780824747));
#18836=CARTESIAN_POINT('Ctrl Pts',(-0.0773044361184472,-0.154747708493488,
0.324878770462053));
#18837=CARTESIAN_POINT('Ctrl Pts',(0.0880972839194656,-0.148868054644337,
0.332817760099358));
#18838=CARTESIAN_POINT('Ctrl Pts',(0.172851978230285,-0.00670989936239309,
0.340756749736664));
#18839=CARTESIAN_POINT('Ctrl Pts',(0.0993725327910066,0.141590708926387,
0.34869573937397));
#18840=CARTESIAN_POINT('Ctrl Pts',(-0.0650756559739905,0.160274727038081,
0.356634729011275));
#18841=CARTESIAN_POINT('Ctrl Pts',(-0.169951541620772,0.0322382168908211,
0.364573718648582));
#18842=CARTESIAN_POINT('Ctrl Pts',(-0.119248438453561,-0.125310171390688,
0.372512708285886));
#18843=CARTESIAN_POINT('Ctrl Pts',(0.0406184374886585,-0.168145685830938,
0.380451697923193));
#18844=CARTESIAN_POINT('Ctrl Pts',(0.163301917673335,-0.0570553486694088,
0.388390687560498));
#18845=CARTESIAN_POINT('Ctrl Pts',(0.136493684039406,0.106265249940549,
0.396329677197804));
#18846=CARTESIAN_POINT('Ctrl Pts',(-0.0152651628095069,0.172307295063139,
0.404268666835109));
#18847=CARTESIAN_POINT('Ctrl Pts',(-0.153049799296248,0.0806138205455782,
0.412207656472416));
#18848=CARTESIAN_POINT('Ctrl Pts',(-0.150727833715048,-0.0848760818555219,
0.420146646109721));
#18849=CARTESIAN_POINT('Ctrl Pts',(-0.0104248664208018,-0.172667748255674,
0.428085635747027));
#18850=CARTESIAN_POINT('Ctrl Pts',(0.139421351618932,-0.10239392482138,
0.436024625384332));
#18851=CARTESIAN_POINT('Ctrl Pts',(0.16163687742079,0.0616145192729195,
0.443963615021638));
#18852=CARTESIAN_POINT('Ctrl Pts',(0.0358849196425865,0.169219093691645,
0.451902604658944));
#18853=CARTESIAN_POINT('Ctrl Pts',(-0.122717222714247,0.121915185177559,
0.45984159429625));
#18854=CARTESIAN_POINT('Ctrl Pts',(-0.168980158036723,-0.0369937199732681,
0.467780583933555));
#18855=CARTESIAN_POINT('Ctrl Pts',(-0.0605533396431397,-0.162037409833775,
0.475719573570861));
#18856=CARTESIAN_POINT('Ctrl Pts',(0.103305911202344,-0.138746956140414,
0.483658563208167));
#18857=CARTESIAN_POINT('Ctrl Pts',(0.172595680358559,0.0115568269495825,
0.491597552845473));
#18858=CARTESIAN_POINT('Ctrl Pts',(0.0838859329010004,0.151281127008313,
0.499536542482778));
#18859=CARTESIAN_POINT('Ctrl Pts',(-0.0816156370489812,0.152517923263679,
0.507475532120084));
#18860=CARTESIAN_POINT('Ctrl Pts',(-0.172403684765527,0.0141350135070757,
0.51541452175739));
#18861=CARTESIAN_POINT('Ctrl Pts',(-0.105367974675403,-0.137187532379513,
0.523353511394695));
#18862=CARTESIAN_POINT('Ctrl Pts',(0.0581248948911363,-0.162924294448283,
0.531292501032001));
#18863=CARTESIAN_POINT('Ctrl Pts',(0.168408406744046,-0.039515030880773,
0.539231490669306));
#18864=CARTESIAN_POINT('Ctrl Pts',(0.124525564004667,0.120067535316156,
0.547170480306613));
#18865=CARTESIAN_POINT('Ctrl Pts',(-0.0333518982867267,0.169736501696743,
0.555109469943918));
#18866=CARTESIAN_POINT('Ctrl Pts',(-0.160697983451488,0.0640233335761385,
0.563048459581225));
#18867=CARTESIAN_POINT('Ctrl Pts',(-0.14093607811848,-0.100298808627811,
0.570987449218529));
#18868=CARTESIAN_POINT('Ctrl Pts',(0.00784314775175556,-0.172804265459278,
0.578926438855836));
#18869=CARTESIAN_POINT('Ctrl Pts',(0.149442509381278,-0.0871192603125336,
0.586865428493141));
#18870=CARTESIAN_POINT('Ctrl Pts',(0.154237495636292,0.0783174569774929,
0.594804418130446));
#18871=CARTESIAN_POINT('Ctrl Pts',(0.0178386252221998,0.172059909850489,
0.602743407767753));
#18872=CARTESIAN_POINT('Ctrl Pts',(-0.134890284021987,0.108293307291099,
0.610682397405058));
#18873=CARTESIAN_POINT('Ctrl Pts',(-0.164136382878957,-0.0546083962682395,
0.618621387042364));
#18874=CARTESIAN_POINT('Ctrl Pts',(-0.0431268722112106,-0.167519855601819,
0.62656037667967));
#18875=CARTESIAN_POINT('Ctrl Pts',(0.117362334288317,-0.127078368017432,
0.634499366316975));
#18876=CARTESIAN_POINT('Ctrl Pts',(0.170414367112955,0.0296946562375699,
0.642438355954282));
#18877=CARTESIAN_POINT('Ctrl Pts',(0.0674637261050104,0.159284257814778,
0.650377345591586));
#18878=CARTESIAN_POINT('Ctrl Pts',(-0.0972453325609638,0.143060037825677,
0.658316335228894));
#18879=CARTESIAN_POINT('Ctrl Pts',(-0.172932953925271,-0.00412584224812367,
0.666255324866198));
#18880=CARTESIAN_POINT('Ctrl Pts',(-0.0903123078403481,-0.147534796506203,
0.674194314503505));
#18881=CARTESIAN_POINT('Ctrl Pts',(0.0749830665657334,-0.155885755782802,
0.68213330414081));
#18882=CARTESIAN_POINT('Ctrl Pts',(0.17163658245605,-0.021533989188811,
0.690072293778116));
#18883=CARTESIAN_POINT('Ctrl Pts',(0.11116857013107,0.132530668686874,0.698011283415421));
#18884=CARTESIAN_POINT('Ctrl Pts',(-0.0510666492692211,0.165272582299639,
0.705950273052727));
#18885=CARTESIAN_POINT('Ctrl Pts',(-0.166553851089581,0.0467187736868841,
0.713889262690032));
#18886=CARTESIAN_POINT('Ctrl Pts',(-0.129572416918314,-0.114602870389546,
0.721828252327339));
#18887=CARTESIAN_POINT('Ctrl Pts',(0.0260236847639906,-0.171013440871999,
0.729767241964644));
#18888=CARTESIAN_POINT('Ctrl Pts',(0.157796886564457,-0.0708729265526718,
0.73770623160195));
#18889=CARTESIAN_POINT('Ctrl Pts',(0.145117853242075,0.0941468947867542,
0.745645221239255));
#18890=CARTESIAN_POINT('Ctrl Pts',(-0.000406629147419015,0.172981686256994,
0.753584210876562));
#18891=CARTESIAN_POINT('Ctrl Pts',(-0.145558870420566,0.0934635991681543,
0.761523200513868));
#18892=CARTESIAN_POINT('Ctrl Pts',(-0.157461941624574,-0.0716140074803496,
0.769462190151172));
#18893=CARTESIAN_POINT('Ctrl Pts',(-0.0252193968429213,-0.17113389830906,
0.777401179788479));
#18894=CARTESIAN_POINT('Ctrl Pts',(0.130109777350283,-0.113992433807847,
0.785340169425784));
#18895=CARTESIAN_POINT('Ctrl Pts',(0.166332367384696,0.0475012914327479,
0.793279159063091));
#18896=CARTESIAN_POINT('Ctrl Pts',(0.0502890745800368,0.165510839842773,
0.801218148700395));
#18897=CARTESIAN_POINT('Ctrl Pts',(-0.111790419467279,0.132006557575396,
0.809157138337702));
#18898=CARTESIAN_POINT('Ctrl Pts',(-0.171533445990104,-0.0223406811520247,
0.817096127975007));
#18899=CARTESIAN_POINT('Ctrl Pts',(-0.0742493586638003,-0.156236557391639,
0.825035117612313));
#18900=CARTESIAN_POINT('Ctrl Pts',(0.0910049278783345,-0.147108572929777,
0.832974107249618));
#18901=CARTESIAN_POINT('Ctrl Pts',(0.172950439922886,-0.00331277195964383,
0.840913096886925));
#18902=CARTESIAN_POINT('Ctrl Pts',(0.0965716772857839,0.143515644700454,
0.848852086524229));
#18903=CARTESIAN_POINT('Ctrl Pts',(-0.0682118374171683,0.158965324406771,
0.856791076161536));
#18904=CARTESIAN_POINT('Ctrl Pts',(-0.170552089827228,0.0288931442238776,
0.864730065798841));
#18905=CARTESIAN_POINT('Ctrl Pts',(-0.116763592698541,-0.127628729319482,
0.872669055436147));
#18906=CARTESIAN_POINT('Ctrl Pts',(0.0439139712140358,-0.167315248138923,
0.880608045073453));
#18907=CARTESIAN_POINT('Ctrl Pts',(0.164391304101163,-0.0538361241500125,
0.888547034710759));
#18908=CARTESIAN_POINT('Ctrl Pts',(0.134379664555536,0.108926281867684,
0.896486024348063));
#18909=CARTESIAN_POINT('Ctrl Pts',(-0.018647348250808,0.17197414204115,
0.904425013985371));
#18910=CARTESIAN_POINT('Ctrl Pts',(-0.154603991719776,0.0775914613336281,
0.912364003622676));
#18911=CARTESIAN_POINT('Ctrl Pts',(-0.149031276472826,-0.0878208845346985,
0.920302993259982));
#18912=CARTESIAN_POINT('Ctrl Pts',(-0.00703064139541984,-0.172839229369798,
0.928241982897287));
#18913=CARTESIAN_POINT('Ctrl Pts',(0.141406064038169,-0.099635105162837,
0.936180972534593));
#18914=CARTESIAN_POINT('Ctrl Pts',(0.160395209035295,0.064778129380991,
0.944119962171899));
#18915=CARTESIAN_POINT('Ctrl Pts',(0.03255353276219,0.169891426011666,0.952058951809204));
#18916=CARTESIAN_POINT('Ctrl Pts',(-0.125088671715395,0.119480765548496,
0.959997941446511));
#18917=CARTESIAN_POINT('Ctrl Pts',(-0.168220770124088,-0.040306347222682,
0.967936931083815));
#18918=CARTESIAN_POINT('Ctrl Pts',(-0.0573582824064844,-0.163195761485875,
0.975875920721122));
#18919=CARTESIAN_POINT('Ctrl Pts',(0.106011781834435,-0.136690640644722,
0.983814910358427));
#18920=CARTESIAN_POINT('Ctrl Pts',(0.17233532526783,0.014945393685262,0.991753899995733));
#18921=CARTESIAN_POINT('Ctrl Pts',(0.0808976893297158,0.152899944371113,
0.999692889633039));
#18922=CARTESIAN_POINT('Ctrl Pts',(-0.0845962369090198,0.150885074902754,
1.00763187927034));
#18923=CARTESIAN_POINT('Ctrl Pts',(-0.172648106016301,0.0107452601904448,
1.01557086890765));
#18924=CARTESIAN_POINT('Ctrl Pts',(-0.102652466413112,-0.13923110380544,
1.02350985854496));
#18925=CARTESIAN_POINT('Ctrl Pts',(0.0613144709582997,-0.161750934398167,
1.03144884818226));
#18926=CARTESIAN_POINT('Ctrl Pts',(0.169152212322519,-0.0361988700648799,
1.03938783781957));
#18927=CARTESIAN_POINT('Ctrl Pts',(0.122142696063681,0.12249077894222,1.04732682745687));
#18928=CARTESIAN_POINT('Ctrl Pts',(-0.0366800874558037,0.169048514669047,
1.05526581709418));
#18929=CARTESIAN_POINT('Ctrl Pts',(-0.161924764760067,0.0608539208677085,
1.06320480673148));
#18930=CARTESIAN_POINT('Ctrl Pts',(-0.138938417355371,-0.103048266896446,
1.07114379636879));
#18931=CARTESIAN_POINT('Ctrl Pts',(0.011236529066559,-0.172616828675865,
1.0790827860061));
#18932=CARTESIAN_POINT('Ctrl Pts',(0.151125203217684,-0.0841665140064042,
1.0870217756434));
#18933=CARTESIAN_POINT('Ctrl Pts',(0.152669111109608,0.0813324759279986,
1.09496076528071));
#18934=CARTESIAN_POINT('Ctrl Pts',(0.0144549108781955,0.172377158228925,
1.10289975491801));
#18935=CARTESIAN_POINT('Ctrl Pts',(-0.136991769602464,0.10562236594946,
1.11083874455532));
#18936=CARTESIAN_POINT('Ctrl Pts',(-0.163031873671196,-0.0578224635832477,
1.11877773419263));
#18937=CARTESIAN_POINT('Ctrl Pts',(-0.0398274706979539,-0.168334790537727,
1.12671672382993));
#18938=CARTESIAN_POINT('Ctrl Pts',(0.119836252144435,-0.124748153491552,
1.13465571346724));
#18939=CARTESIAN_POINT('Ctrl Pts',(0.169798099063322,0.0330368685268242,
1.14259470310454));
#18940=CARTESIAN_POINT('Ctrl Pts',(0.0643214233134591,0.160578901573361,
1.15053369274185));
#18941=CARTESIAN_POINT('Ctrl Pts',(-0.100037107244844,0.141121955420339,
1.15847268237915));
#18942=CARTESIAN_POINT('Ctrl Pts',(-0.172818522111203,-0.00752246920075927,
1.16641167201646));
#18943=CARTESIAN_POINT('Ctrl Pts',(-0.0873964240115842,-0.149280588817046,
1.17435066165376));
#18944=CARTESIAN_POINT('Ctrl Pts',(0.0780311106025284,-0.154382560238235,
1.18228965129107));
#18945=CARTESIAN_POINT('Ctrl Pts',(0.172026511281289,-0.01815787828917,
1.19022864092837));
#18946=CARTESIAN_POINT('Ctrl Pts',(0.10854343062882,0.134689096792963,1.19816763056568));
#18947=CARTESIAN_POINT('Ctrl Pts',(-0.0543037217972188,0.164237434607784,
1.20610662020299));
#18948=CARTESIAN_POINT('Ctrl Pts',(-0.167439538594998,0.0434376569656869,
1.21404560984029));
#18949=CARTESIAN_POINT('Ctrl Pts',(-0.127295933190098,-0.117126318651471,
1.2219845994776));
#18950=CARTESIAN_POINT('Ctrl Pts',(0.0293783748903316,-0.170469176734012,
1.2299235891149));
#18951=CARTESIAN_POINT('Ctrl Pts',(0.159158794190081,-0.0677591865323411,
1.23786257875221));
#18952=CARTESIAN_POINT('Ctrl Pts',(0.143240245273553,0.0969796950995427,
1.24580156838952));
#18953=CARTESIAN_POINT('Ctrl Pts',(-0.00380493129617075,0.172940312320012,
1.25374055802682));
#18954=CARTESIAN_POINT('Ctrl Pts',(-0.147366954032488,0.0905859259858403,
1.26167954766413));
#18955=CARTESIAN_POINT('Ctrl Pts',(-0.156024630070406,-0.074693667330688,
1.26961853730143));
#18956=CARTESIAN_POINT('Ctrl Pts',(-0.0218524503424686,-0.171596327294885,
1.27755752693874));
#18957=CARTESIAN_POINT('Ctrl Pts',(0.132324150022753,-0.111414309889572,
1.28549651657604));
#18958=CARTESIAN_POINT('Ctrl Pts',(0.165367059817933,0.0507598725070622,
1.29343550621335));
#18959=CARTESIAN_POINT('Ctrl Pts',(0.0470277596764783,0.166466870408131,
1.30137449585065));
#18960=CARTESIAN_POINT('Ctrl Pts',(-0.114362231391601,0.129784857201791,
1.30931348548797));
#18961=CARTESIAN_POINT('Ctrl Pts',(-0.171061437441431,-0.0257062980954763,
1.31725247512526));
#18962=CARTESIAN_POINT('Ctrl Pts',(-0.071165620995849,-0.157665099140374,
1.32519146476257));
#18963=CARTESIAN_POINT('Ctrl Pts',(0.0938774439379855,-0.145292307632914,
1.33313045439988));
#18964=CARTESIAN_POINT('Ctrl Pts',(0.172982143233999,8.56343898915854E-5,
1.34106944403719));
#18965=CARTESIAN_POINT('Ctrl Pts',(0.0937335447930804,0.145385183220099,
1.34900843367449));
#18966=CARTESIAN_POINT('Ctrl Pts',(-0.0713216883190155,0.157594562185848,
1.3569474233118));
#18967=CARTESIAN_POINT('Ctrl Pts',(-0.171086806821499,0.0255369173285507,
1.3648864129491));
#18968=CARTESIAN_POINT('Ctrl Pts',(-0.114233673229396,-0.129898019862958,
1.37282540258641));
#18969=CARTESIAN_POINT('Ctrl Pts',(0.0471925482590101,-0.166420232464351,
1.38076439222371));
#18970=CARTESIAN_POINT('Ctrl Pts',(0.165417247017141,-0.0505961085897048,
1.38870338186102));
#18971=CARTESIAN_POINT('Ctrl Pts',(0.132213753266125,0.111545248710567,
1.39664237149832));
#18972=CARTESIAN_POINT('Ctrl Pts',(-0.0220222951247444,0.17157464463752,
1.40458136113563));
#18973=CARTESIAN_POINT('Ctrl Pts',(-0.156098584526576,0.0745390809398717,
1.41252035077293));
#18974=CARTESIAN_POINT('Ctrl Pts',(-0.147277046608992,-0.0907316537045687,
1.42045934041024));
#18975=CARTESIAN_POINT('Ctrl Pts',(-0.00363398118293899,-0.172944250658386,
1.42839833004755));
#18976=CARTESIAN_POINT('Ctrl Pts',(0.143336722904634,-0.0968373407211472,
1.43633731968485));
#18977=CARTESIAN_POINT('Ctrl Pts',(0.159090624036536,0.0679158129692223,
1.44427630932216));
#18978=CARTESIAN_POINT('Ctrl Pts',(0.0292114869387437,0.170499931406899,
1.45221529895946));
#18979=CARTESIAN_POINT('Ctrl Pts',(-0.127415456569397,0.116996902323752,
1.46015428859677));
#18980=CARTESIAN_POINT('Ctrl Pts',(-0.167389576437263,-0.0435971050111283,
1.46809327823408));
#18981=CARTESIAN_POINT('Ctrl Pts',(-0.0541541359620402,-0.164303103757731,
1.47603226787138));
#18982=CARTESIAN_POINT('Ctrl Pts',(0.108701533888403,-0.13455879509903,
1.48397125750869));
#18983=CARTESIAN_POINT('Ctrl Pts',(0.171961157005542,0.0182848320604298,
1.49191024714599));
#18984=CARTESIAN_POINT('Ctrl Pts',(0.0779697431325927,0.154543202561513,
1.4998492367833));
#18985=CARTESIAN_POINT('Ctrl Pts',(-0.0877325682749983,0.149025855561406,
1.5077882264206));
#18986=CARTESIAN_POINT('Ctrl Pts',(-0.144149484752264,0.0548439265155397,
1.51308088617881));
#18987=CARTESIAN_POINT('Ctrl Pts',(-0.146217781693078,0.00621955116994065,
1.51572721605791));
#18988=CARTESIAN_POINT('Ctrl Pts',(0.0795408277542855,-0.111329858282327,
-0.0109985226280624));
#18989=CARTESIAN_POINT('Ctrl Pts',(0.116563307192903,-0.0848787452970238,
-0.00835219274896048));
#18990=CARTESIAN_POINT('Ctrl Pts',(0.16150817751539,0.00739908052493189,
-0.00305953299075667));
#18991=CARTESIAN_POINT('Ctrl Pts',(0.0812084309002137,0.139981433724326,
0.00487945664654907));
#18992=CARTESIAN_POINT('Ctrl Pts',(-0.0734975292821143,0.144003850402812,
0.0128184462838548));
#18993=CARTESIAN_POINT('Ctrl Pts',(-0.160887120581772,0.0164101388376342,
0.0207574359211605));
#18994=CARTESIAN_POINT('Ctrl Pts',(-0.101013704785435,-0.126315124179183,
0.0286964255584662));
#18995=CARTESIAN_POINT('Ctrl Pts',(0.0513403816191153,-0.153350170642076,
0.0366354151957719));
#18996=CARTESIAN_POINT('Ctrl Pts',(0.156690838735662,-0.0400338514845966,
0.0445744048330777));
#18997=CARTESIAN_POINT('Ctrl Pts',(0.118604220350264,0.109946623274354,
0.0525133944703833));
#18998=CARTESIAN_POINT('Ctrl Pts',(-0.0280578283917351,0.15927012049393,
0.0604523841076892));
#18999=CARTESIAN_POINT('Ctrl Pts',(-0.14903412333264,0.0627971513379326,
0.0683913737449947));
#19000=CARTESIAN_POINT('Ctrl Pts',(-0.133580279395553,-0.0911646307683348,
0.0763303633823007));
#19001=CARTESIAN_POINT('Ctrl Pts',(0.0041573593468571,-0.161670216863261,
0.0842693530196062));
#19002=CARTESIAN_POINT('Ctrl Pts',(0.138089113144455,-0.0841784443595545,
0.0922083426569122));
#19003=CARTESIAN_POINT('Ctrl Pts',(0.14560980428584,0.0703732645446943,
0.100147332294218));
#19004=CARTESIAN_POINT('Ctrl Pts',(0.0198346691022095,0.160502893816501,
0.108086321931524));
#19005=CARTESIAN_POINT('Ctrl Pts',(-0.124097730593135,0.103703218031488,
0.116025311568829));
#19006=CARTESIAN_POINT('Ctrl Pts',(-0.154427171169137,-0.0480296962598115,
0.123964301206135));
#19007=CARTESIAN_POINT('Ctrl Pts',(-0.0433891157712434,-0.155794689166463,
0.13190329084344));
#19008=CARTESIAN_POINT('Ctrl Pts',(0.107368699171666,-0.12094033522185,
0.139842280480747));
#19009=CARTESIAN_POINT('Ctrl Pts',(0.15983782968835,0.0246266142906177,
0.147781270118052));
#19010=CARTESIAN_POINT('Ctrl Pts',(0.0659863808909888,0.147649582370873,
0.155720259755358));
#19011=CARTESIAN_POINT('Ctrl Pts',(-0.0882710769349216,0.135509478890084,
0.163659249392663));
#19012=CARTESIAN_POINT('Ctrl Pts',(-0.161722413615419,-0.00068026650363694,
0.171598239029969));
#19013=CARTESIAN_POINT('Ctrl Pts',(-0.0871279640988751,-0.136247273976568,
0.179537228667275));
#19014=CARTESIAN_POINT('Ctrl Pts',(0.0672261652318651,-0.147089240053593,
0.187476218304581));
#19015=CARTESIAN_POINT('Ctrl Pts',(0.160039347628626,-0.023281087390596,
0.195415207941886));
#19016=CARTESIAN_POINT('Ctrl Pts',(0.106347475470598,0.121839305139765,
0.203354197579192));
#19017=CARTESIAN_POINT('Ctrl Pts',(-0.0446982220051161,0.15542416405057,
0.211293187216498));
#19018=CARTESIAN_POINT('Ctrl Pts',(-0.154825760608133,0.0467288526640558,
0.219232176853804));
#19019=CARTESIAN_POINT('Ctrl Pts',(-0.12322092627477,-0.104743520787053,
0.227171166491109));
#19020=CARTESIAN_POINT('Ctrl Pts',(0.0211842211805034,-0.160330379506191,
0.235110156128415));
#19021=CARTESIAN_POINT('Ctrl Pts',(0.146196665995071,-0.0691457639426259,
0.24304914576572));
#19022=CARTESIAN_POINT('Ctrl Pts',(0.137376082602736,0.0853370596399817,
0.250988135403027));
#19023=CARTESIAN_POINT('Ctrl Pts',(0.00279711058556459,0.161699653653757,
0.258927125040332));
#19024=CARTESIAN_POINT('Ctrl Pts',(-0.134342424474264,0.0900372967480426,
0.266866114677638));
#19025=CARTESIAN_POINT('Ctrl Pts',(-0.148500677015507,-0.0640480346713102,
0.274805104314944));
#19026=CARTESIAN_POINT('Ctrl Pts',(-0.0267167371651392,-0.159501779847699,
0.282744093952249));
#19027=CARTESIAN_POINT('Ctrl Pts',(0.119524544542348,-0.108942576944327,
0.290683083589556));
#19028=CARTESIAN_POINT('Ctrl Pts',(0.156349297273321,0.0413460888291301,
0.29862207322686));
#19029=CARTESIAN_POINT('Ctrl Pts',(0.0500469836677093,0.153785243912065,
0.306561062864167));
#19030=CARTESIAN_POINT('Ctrl Pts',(-0.102069913541897,0.125444547784578,
0.314500052501472));
#19031=CARTESIAN_POINT('Ctrl Pts',(-0.160748800211922,-0.0177320345633525,
0.322439042138778));
#19032=CARTESIAN_POINT('Ctrl Pts',(-0.0722731771226978,-0.144676154524232,
0.330378031776084));
#19033=CARTESIAN_POINT('Ctrl Pts',(0.082363586418043,-0.139179170322594,
0.338317021413389));
#19034=CARTESIAN_POINT('Ctrl Pts',(0.16160213133829,-0.00627319426210969,
0.346256011050695));
#19035=CARTESIAN_POINT('Ctrl Pts',(0.0929050003357002,0.132375461215256,
0.354195000688001));
#19036=CARTESIAN_POINT('Ctrl Pts',(-0.0608402912787218,0.149843454232904,
0.362133990325306));
#19037=CARTESIAN_POINT('Ctrl Pts',(-0.158890465884947,0.0301400343429239,
0.370072979962613));
#19038=CARTESIAN_POINT('Ctrl Pts',(-0.1114873084483,-0.117154521356547,
0.378011969599918));
#19039=CARTESIAN_POINT('Ctrl Pts',(0.0379748391485164,-0.157202141877815,
0.385950959237223));
#19040=CARTESIAN_POINT('Ctrl Pts',(0.152673624090564,-0.0533419752763387,
0.39388994887453));
#19041=CARTESIAN_POINT('Ctrl Pts',(0.127610169584502,0.0993491139263089,
0.401828938511835));
#19042=CARTESIAN_POINT('Ctrl Pts',(-0.014271649480085,0.16109289816887,
0.409767928149142));
#19043=CARTESIAN_POINT('Ctrl Pts',(-0.143088751545671,0.0753671745551693,
0.417706917786446));
#19044=CARTESIAN_POINT('Ctrl Pts',(-0.140917908083783,-0.0793520321139836,
0.425645907423752));
#19045=CARTESIAN_POINT('Ctrl Pts',(-0.00974637750615997,-0.161429891732714,
0.433584897061058));
#19046=CARTESIAN_POINT('Ctrl Pts',(0.130347293715478,-0.0957297489831606,
0.441523886698364));
#19047=CARTESIAN_POINT('Ctrl Pts',(0.15111695082405,0.0576044181723055,
0.449462876335669));
#19048=CARTESIAN_POINT('Ctrl Pts',(0.0335493961742207,0.158205688379633,
0.457401865972975));
#19049=CARTESIAN_POINT('Ctrl Pts',(-0.114730331382826,0.113980493419335,
0.465340855610281));
#19050=CARTESIAN_POINT('Ctrl Pts',(-0.157982303542021,-0.03458603167299,
0.473279845247587));
#19051=CARTESIAN_POINT('Ctrl Pts',(-0.0566123040428622,-0.151491415104245,
0.481218834884892));
#19052=CARTESIAN_POINT('Ctrl Pts',(0.0965823799129518,-0.129716790392294,
0.489157824522198));
#19053=CARTESIAN_POINT('Ctrl Pts',(0.161362514281243,0.0108046658515635,
0.497096814159504));
#19054=CARTESIAN_POINT('Ctrl Pts',(0.0784263257203939,0.141435191000425,
0.50503580379681));
#19055=CARTESIAN_POINT('Ctrl Pts',(-0.076303789130349,0.14259149197508,
0.512974793434115));
#19056=CARTESIAN_POINT('Ctrl Pts',(-0.161183014472451,0.0132150544797126,
0.520913783071421));
#19057=CARTESIAN_POINT('Ctrl Pts',(-0.0985102366584373,-0.128258859705,
0.528852772708727));
#19058=CARTESIAN_POINT('Ctrl Pts',(0.0543419114689404,-0.152320577983508,
0.536791762346032));
#19059=CARTESIAN_POINT('Ctrl Pts',(0.157447763940923,-0.0369432463290883,
0.544730751983338));
#19060=CARTESIAN_POINT('Ctrl Pts',(0.116420979124965,0.112253095453589,
0.552669741620643));
#19061=CARTESIAN_POINT('Ctrl Pts',(-0.0311812332291155,0.158689421555565,
0.56060873125795));
#19062=CARTESIAN_POINT('Ctrl Pts',(-0.150239163551416,0.0598564579197502,
0.568547720895255));
#19063=CARTESIAN_POINT('Ctrl Pts',(-0.131763436204723,-0.0937709907106254,
0.576486710532561));
#19064=CARTESIAN_POINT('Ctrl Pts',(0.00733268664935855,-0.161557523891122,
0.584425700169866));
#19065=CARTESIAN_POINT('Ctrl Pts',(0.139716237417787,-0.0814492162095161,
0.592364689807173));
#19066=CARTESIAN_POINT('Ctrl Pts',(0.144199148209332,0.0732202668325601,
0.600303679444478));
#19067=CARTESIAN_POINT('Ctrl Pts',(0.0166776214282734,0.160861613702037,
0.608242669081784));
#19068=CARTESIAN_POINT('Ctrl Pts',(-0.126111124778327,0.101245177793678,
0.616181658719089));
#19069=CARTESIAN_POINT('Ctrl Pts',(-0.153453779210204,-0.0510542795996006,
0.624120648356396));
#19070=CARTESIAN_POINT('Ctrl Pts',(-0.0403200156494649,-0.156617042997737,
0.6320596379937));
#19071=CARTESIAN_POINT('Ctrl Pts',(0.10972395892722,-0.118807637198397,
0.639998627631007));
#19072=CARTESIAN_POINT('Ctrl Pts',(0.159323168980049,0.0277620180369333,
0.647937617268312));
#19073=CARTESIAN_POINT('Ctrl Pts',(0.0630729369615192,0.148917448414806,
0.655876606905618));
#19074=CARTESIAN_POINT('Ctrl Pts',(-0.0909162461746061,0.133749160748195,
0.663815596542924));
#19075=CARTESIAN_POINT('Ctrl Pts',(-0.161677836835157,-0.00385731715476066,
0.671754586180229));
#19076=CARTESIAN_POINT('Ctrl Pts',(-0.0844344483789265,-0.137932685561743,
0.679693575817536));
#19077=CARTESIAN_POINT('Ctrl Pts',(0.0701028908975481,-0.145740133481257,
0.687632565454841));
#19078=CARTESIAN_POINT('Ctrl Pts',(0.1604658380222,-0.0201324774223393,
0.695571555092147));
#19079=CARTESIAN_POINT('Ctrl Pts',(0.10393330787963,0.123905081947942,0.703510544729453));
#19080=CARTESIAN_POINT('Ctrl Pts',(-0.0477430426119635,0.15451603056473,
0.711449534366758));
#19081=CARTESIAN_POINT('Ctrl Pts',(-0.155713909636705,0.0436781428746717,
0.719388524004064));
#19082=CARTESIAN_POINT('Ctrl Pts',(-0.121139364160222,-0.10714409115852,
0.72732751364137));
#19083=CARTESIAN_POINT('Ctrl Pts',(0.0243299669821161,-0.159883252800214,
0.735266503278675));
#19084=CARTESIAN_POINT('Ctrl Pts',(0.147526880793862,-0.0662602540182413,
0.743205492915981));
#19085=CARTESIAN_POINT('Ctrl Pts',(0.135673045916277,0.0880194662056535,
0.751144482553287));
#19086=CARTESIAN_POINT('Ctrl Pts',(-0.000380164216571841,0.161723397486253,
0.759083472190592));
#19087=CARTESIAN_POINT('Ctrl Pts',(-0.136085360063504,0.0873806419964673,
0.767022461827899));
#19088=CARTESIAN_POINT('Ctrl Pts',(-0.147213735311121,-0.0669531026545853,
0.774961451465203));
#19089=CARTESIAN_POINT('Ctrl Pts',(-0.023578025097595,-0.159995870421162,
0.78290044110251));
#19090=CARTESIAN_POINT('Ctrl Pts',(0.121641751185188,-0.106573384050283,
0.790839430739816));
#19091=CARTESIAN_POINT('Ctrl Pts',(0.155506840911589,0.0444097314676148,
0.798778420377121));
#19092=CARTESIAN_POINT('Ctrl Pts',(0.047016075363265,0.15473878142458,0.806717410014428));
#19093=CARTESIAN_POINT('Ctrl Pts',(-0.104514684958047,0.123415081928621,
0.814656399651731));
#19094=CARTESIAN_POINT('Ctrl Pts',(-0.16036941405942,-0.020886666885039,
0.82259538928904));
#19095=CARTESIAN_POINT('Ctrl Pts',(-0.0694169354231278,-0.146068103622213,
0.830534378926343));
#19096=CARTESIAN_POINT('Ctrl Pts',(0.085081990139753,-0.137534202194171,
0.838473368563651));
#19097=CARTESIAN_POINT('Ctrl Pts',(0.161694184779289,-0.00309716449182502,
0.846412358200955));
#19098=CARTESIAN_POINT('Ctrl Pts',(0.0902864348795877,0.134175115040242,
0.854351347838261));
#19099=CARTESIAN_POINT('Ctrl Pts',(-0.0637723584188847,0.148619272374149,
0.862290337475567));
#19100=CARTESIAN_POINT('Ctrl Pts',(-0.159451928190027,0.0270126713934565,
0.870229327112872));
#19101=CARTESIAN_POINT('Ctrl Pts',(-0.109164185657521,-0.119322178948671,
0.878168316750179));
#19102=CARTESIAN_POINT('Ctrl Pts',(0.0410558873341998,-0.156425752146281,
0.886107306387484));
#19103=CARTESIAN_POINT('Ctrl Pts',(0.153692109215179,-0.0503322698109037,
0.894046296024789));
#19104=CARTESIAN_POINT('Ctrl Pts',(0.125633738317809,0.101836956040625,
0.901985285662096));
#19105=CARTESIAN_POINT('Ctrl Pts',(-0.0174337097671096,0.160781427979367,
0.909924275299401));
#19106=CARTESIAN_POINT('Ctrl Pts',(-0.144541791370401,0.072541521673891,
0.917863264936708));
#19107=CARTESIAN_POINT('Ctrl Pts',(-0.13933176907,-0.082105176128868,0.925802254574012));
#19108=CARTESIAN_POINT('Ctrl Pts',(-0.00657306121577474,-0.161590212220858,
0.933741244211319));
#19109=CARTESIAN_POINT('Ctrl Pts',(0.132202833700187,-0.0931504835251481,
0.941680233848624));
#19110=CARTESIAN_POINT('Ctrl Pts',(0.149956094815541,0.0605621288182698,
0.949619223485929));
#19111=CARTESIAN_POINT('Ctrl Pts',(0.0304348282896272,0.158834262822317,
0.957558213123236));
#19112=CARTESIAN_POINT('Ctrl Pts',(-0.116947437700435,0.111704514835484,
0.965497202760542));
#19113=CARTESIAN_POINT('Ctrl Pts',(-0.157272339407096,-0.0376830608728604,
0.973436192397847));
#19114=CARTESIAN_POINT('Ctrl Pts',(-0.0536251929639052,-0.152574376940928,
0.981375182035153));
#19115=CARTESIAN_POINT('Ctrl Pts',(0.0991121424632477,-0.127794307524525,
0.989314171672459));
#19116=CARTESIAN_POINT('Ctrl Pts',(0.161119104064031,0.0139726921146952,
0.997253161309763));
#19117=CARTESIAN_POINT('Ctrl Pts',(0.0756325681075411,0.142948649734045,
1.00519215094707));
#19118=CARTESIAN_POINT('Ctrl Pts',(-0.0790904005129918,0.141064915432658,
1.01313114058437));
#19119=CARTESIAN_POINT('Ctrl Pts',(-0.161411527883023,0.0100459188627121,
1.02107013022168));
#19120=CARTESIAN_POINT('Ctrl Pts',(-0.095971463730607,-0.130169427934261,
1.02900911985899));
#19121=CARTESIAN_POINT('Ctrl Pts',(0.0573238981132153,-0.151223584550935,
1.03694810949629));
#19122=CARTESIAN_POINT('Ctrl Pts',(0.158143159897702,-0.0338429135403315,
1.0448870991336));
#19123=CARTESIAN_POINT('Ctrl Pts',(0.114193197054413,0.114518625410106,
1.0528260887709));
#19124=CARTESIAN_POINT('Ctrl Pts',(-0.0342928115212847,0.158046211271557,
1.06076507840821));
#19125=CARTESIAN_POINT('Ctrl Pts',(-0.151386101389109,0.0568933223281485,
1.06870406804552));
#19126=CARTESIAN_POINT('Ctrl Pts',(-0.129895790602315,-0.0963415040526547,
1.07664305768282));
#19127=CARTESIAN_POINT('Ctrl Pts',(0.0105052141409744,-0.161382286187737,
1.08458204732013));
#19128=CARTESIAN_POINT('Ctrl Pts',(0.141289415307547,-0.0786886455683398,
1.09252103695743));
#19129=CARTESIAN_POINT('Ctrl Pts',(0.14273283995608,0.076039057183793,1.10046002659474));
#19130=CARTESIAN_POINT('Ctrl Pts',(0.013514131745196,0.161158214381091,
1.10839901623204));
#19131=CARTESIAN_POINT('Ctrl Pts',(-0.128075837894479,0.0987480712062529,
1.11633800586935));
#19132=CARTESIAN_POINT('Ctrl Pts',(-0.152421155552179,-0.0540591635106084,
1.12427699550666));
#19133=CARTESIAN_POINT('Ctrl Pts',(-0.0372353514058616,-0.157378938949945,
1.13221598514396));
#19134=CARTESIAN_POINT('Ctrl Pts',(0.11203686504723,-0.116629081663695,
1.14015497478127));
#19135=CARTESIAN_POINT('Ctrl Pts',(0.158747009937404,0.0308867067726846,
1.14809396441857));
#19136=CARTESIAN_POINT('Ctrl Pts',(0.0601351468730053,0.150127831962932,
1.15603295405588));
#19137=CARTESIAN_POINT('Ctrl Pts',(-0.0935263218228598,0.13193721592339,
1.16397194369318));
#19138=CARTESIAN_POINT('Ctrl Pts',(-0.161570852667341,-0.00703287904607843,
1.17191093333049));
#19139=CARTESIAN_POINT('Ctrl Pts',(-0.0817083410685703,-0.13956485524354,
1.17984992296779));
#19140=CARTESIAN_POINT('Ctrl Pts',(0.0729525569401478,-0.144334771469742,
1.1877889126051));
#19141=CARTESIAN_POINT('Ctrl Pts',(0.160830388835411,-0.016976096323307,
1.19572790224241));
#19142=CARTESIAN_POINT('Ctrl Pts',(0.101479022178261,0.125923031559255,
1.20366689187971));
#19143=CARTESIAN_POINT('Ctrl Pts',(-0.0507694344715009,0.153548254118279,
1.21160588151702));
#19144=CARTESIAN_POINT('Ctrl Pts',(-0.15654195331917,0.0406105733811438,
1.21954487115432));
#19145=CARTESIAN_POINT('Ctrl Pts',(-0.119011042423884,-0.109503304062093,
1.22748386079163));
#19146=CARTESIAN_POINT('Ctrl Pts',(0.0274663214511058,-0.159374411387982,
1.23542285042894));
#19147=CARTESIAN_POINT('Ctrl Pts',(0.148800150427453,-0.0633491677300162,
1.24336184006624));
#19148=CARTESIAN_POINT('Ctrl Pts',(0.133917639627974,0.0906678973829495,
1.25130082970354));
#19149=CARTESIAN_POINT('Ctrl Pts',(-0.00355729227603857,0.161684716318317,
1.25923981934086));
#19150=CARTESIAN_POINT('Ctrl Pts',(-0.137775766897813,0.0846902584421788,
1.26717880897816));
#19151=CARTESIAN_POINT('Ctrl Pts',(-0.14586996931591,-0.0698323268364953,
1.27511779861547));
#19152=CARTESIAN_POINT('Ctrl Pts',(-0.0204302119447119,-0.160428202816007,
1.28305678825277));
#19153=CARTESIAN_POINT('Ctrl Pts',(0.123712004283314,-0.104163053984564,
1.29099577789008));
#19154=CARTESIAN_POINT('Ctrl Pts',(0.15460435913624,0.0474562320176185,
1.29893476752738));
#19155=CARTESIAN_POINT('Ctrl Pts',(0.043967018911749,0.155632589980133,
1.30687375716469));
#19156=CARTESIAN_POINT('Ctrl Pts',(-0.106919113837756,0.121337978043289,
1.31481274680199));
#19157=CARTESIAN_POINT('Ctrl Pts',(-0.159928125575155,-0.0240332370134145,
1.3227517364393));
#19158=CARTESIAN_POINT('Ctrl Pts',(-0.0665338988230771,-0.147403670583407,
1.33069072607661));
#19159=CARTESIAN_POINT('Ctrl Pts',(0.0877675522160205,-0.135836146169277,
1.33862971571391));
#19160=CARTESIAN_POINT('Ctrl Pts',(0.161723824721502,8.00609866524728E-5,
1.34656870535122));
#19161=CARTESIAN_POINT('Ctrl Pts',(0.0876330185603928,0.135922977069285,
1.35450769498852));
#19162=CARTESIAN_POINT('Ctrl Pts',(-0.0666798087068602,0.147337724435113,
1.36244668462583));
#19163=CARTESIAN_POINT('Ctrl Pts',(-0.159951843822013,0.0238748801740983,
1.37038567426313));
#19164=CARTESIAN_POINT('Ctrl Pts',(-0.106798922716859,-0.121443775659372,
1.37832466390044));
#19165=CARTESIAN_POINT('Ctrl Pts',(0.0441210824430389,-0.155588987406456,
1.38626365353774));
#19166=CARTESIAN_POINT('Ctrl Pts',(0.154651279966657,-0.0473031264624986,
1.39420264317505));
#19167=CARTESIAN_POINT('Ctrl Pts',(0.123608792556459,0.10428547082216,1.40214163281236));
#19168=CARTESIAN_POINT('Ctrl Pts',(-0.020589002599541,0.160407931346284,
1.41008062244966));
#19169=CARTESIAN_POINT('Ctrl Pts',(-0.145939110542184,0.0696878015005003,
1.41801961208697));
#19170=CARTESIAN_POINT('Ctrl Pts',(-0.137691710982408,-0.0848265016612731,
1.42595860172427));
#19171=CARTESIAN_POINT('Ctrl Pts',(-0.00339746822928561,-0.161688398335044,
1.43389759136158));
#19172=CARTESIAN_POINT('Ctrl Pts',(0.134007838137522,-0.0905348079547059,
1.44183658099889));
#19173=CARTESIAN_POINT('Ctrl Pts',(0.148736417039967,0.0634956003383226,
1.44977557063619));
#19174=CARTESIAN_POINT('Ctrl Pts',(0.0273102951854726,0.159403164432859,
1.4577145602735));
#19175=CARTESIAN_POINT('Ctrl Pts',(-0.119122786779006,0.109382310628272,
1.4656535499108));
#19176=CARTESIAN_POINT('Ctrl Pts',(-0.156495242883694,-0.0407596439572756,
1.47359253954811));
#19177=CARTESIAN_POINT('Ctrl Pts',(-0.0506295842364637,-0.153609649276743,
1.48153152918541));
#19178=CARTESIAN_POINT('Ctrl Pts',(0.10162683549218,-0.125801210382132,
1.48947051882272));
#19179=CARTESIAN_POINT('Ctrl Pts',(0.160769288057966,0.017094787472962,
1.49740950846002));
#19180=CARTESIAN_POINT('Ctrl Pts',(0.0728951834924312,0.144484958595688,
1.50534849809733));
#19181=CARTESIAN_POINT('Ctrl Pts',(-0.0820226078184241,0.139326700971572,
1.51328748773464));
#19182=CARTESIAN_POINT('Ctrl Pts',(-0.134767702434085,0.0512744806661359,
1.51858014749284));
#19183=CARTESIAN_POINT('Ctrl Pts',(-0.136701386950156,0.00581475974600206,
1.52122647737194));
#19184=CARTESIAN_POINT('Ctrl Pts',(0.0740036351041134,-0.103579689087085,
-0.0054992613140312));
#19185=CARTESIAN_POINT('Ctrl Pts',(0.108448814220036,-0.0789699563406641,
-0.00285293143492929));
#19186=CARTESIAN_POINT('Ctrl Pts',(0.150264871169078,0.00688399744800666,
0.00243972832327453));
#19187=CARTESIAN_POINT('Ctrl Pts',(0.0755551489391376,0.130236700260234,
0.0103787179605803));
#19188=CARTESIAN_POINT('Ctrl Pts',(-0.0683810376584167,0.133979098529349,
0.0183177075978859));
#19189=CARTESIAN_POINT('Ctrl Pts',(-0.14968704878538,0.0152677557027674,
0.0262566972351917));
#19190=CARTESIAN_POINT('Ctrl Pts',(-0.0939816891590436,-0.11752176362514,
0.0341956868724974));
#19191=CARTESIAN_POINT('Ctrl Pts',(0.0477663481097245,-0.142674779628989,
0.0421346765098031));
#19192=CARTESIAN_POINT('Ctrl Pts',(0.14578288888032,-0.0372469160898187,
0.0500736661471088));
#19193=CARTESIAN_POINT('Ctrl Pts',(0.110347650287512,0.102292747252513,
0.0580126557844146));
#19194=CARTESIAN_POINT('Ctrl Pts',(-0.0261045975097209,0.148182615303324,
0.0659516454217203));
#19195=CARTESIAN_POINT('Ctrl Pts',(-0.13865919166998,0.0584255608647477,
0.073890635059026));
#19196=CARTESIAN_POINT('Ctrl Pts',(-0.124281158904105,-0.0848182532198701,
0.0818296246963318));
#19197=CARTESIAN_POINT('Ctrl Pts',(0.00386794697500161,-0.15041563023346,
0.0897686143336374));
#19198=CARTESIAN_POINT('Ctrl Pts',(0.128476112576568,-0.0783184064825255,
0.0977076039709433));
#19199=CARTESIAN_POINT('Ctrl Pts',(0.135473254782295,0.0654742669580799,
0.105646593608249));
#19200=CARTESIAN_POINT('Ctrl Pts',(0.0184538891044151,0.149329569763132,
0.113585583245555));
#19201=CARTESIAN_POINT('Ctrl Pts',(-0.115458732720671,0.096483973363118,
0.12152457288286));
#19202=CARTESIAN_POINT('Ctrl Pts',(-0.143676805334049,-0.0446861343604874,
0.129463562520166));
#19203=CARTESIAN_POINT('Ctrl Pts',(-0.0403686054279526,-0.144949124289353,
0.137402552157472));
#19204=CARTESIAN_POINT('Ctrl Pts',(0.0998942839726139,-0.112521137758025,
0.145341541794778));
#19205=CARTESIAN_POINT('Ctrl Pts',(0.14871080372247,0.0229122455632766,
0.153280531432083));
#19206=CARTESIAN_POINT('Ctrl Pts',(0.0613927738894439,0.137371034794898,
0.161219521069389));
#19207=CARTESIAN_POINT('Ctrl Pts',(-0.0821261326059948,0.126076058196294,
0.169158510706695));
#19208=CARTESIAN_POINT('Ctrl Pts',(-0.150464193336327,-0.000632910110818063,
0.177097500344));
#19209=CARTESIAN_POINT('Ctrl Pts',(-0.0810625969653723,-0.126762492068094,
0.185036489981306));
#19210=CARTESIAN_POINT('Ctrl Pts',(0.0625462512992226,-0.136849700411639,
0.192975479618612));
#19211=CARTESIAN_POINT('Ctrl Pts',(0.148898293097928,-0.0216603868066741,
0.200914469255917));
#19212=CARTESIAN_POINT('Ctrl Pts',(0.0989441522193119,0.113357526360621,
0.208853458893223));
#19213=CARTESIAN_POINT('Ctrl Pts',(-0.0415865789238149,0.144604393083411,
0.216792448530529));
#19214=CARTESIAN_POINT('Ctrl Pts',(-0.144047647180085,0.0434758483035601,
0.224731438167835));
#19215=CARTESIAN_POINT('Ctrl Pts',(-0.114642966671137,-0.0974518559926297,
0.232670427805141));
#19216=CARTESIAN_POINT('Ctrl Pts',(0.0197094928286333,-0.149169064945282,
0.240609417442446));
#19217=CARTESIAN_POINT('Ctrl Pts',(0.136019262424063,-0.0643322181611298,
0.248548407079752));
#19218=CARTESIAN_POINT('Ctrl Pts',(0.127812719278849,0.0793963653730636,
0.256487396717058));
#19219=CARTESIAN_POINT('Ctrl Pts',(0.00260239121171357,0.150443017797356,
0.264426386354363));
#19220=CARTESIAN_POINT('Ctrl Pts',(-0.124990247656303,0.0837693979610897,
0.272365375991669));
#19221=CARTESIAN_POINT('Ctrl Pts',(-0.138162880936044,-0.0595893646165358,
0.280304365628975));
#19222=CARTESIAN_POINT('Ctrl Pts',(-0.0248568656394851,-0.148398147813718,
0.288243355266281));
#19223=CARTESIAN_POINT('Ctrl Pts',(0.111203906597776,-0.101358597076653,
0.296182344903586));
#19224=CARTESIAN_POINT('Ctrl Pts',(0.145465123646218,0.0384678027257296,
0.304121334540892));
#19225=CARTESIAN_POINT('Ctrl Pts',(0.0465629893725541,0.143079565503422,
0.312060324178198));
#19226=CARTESIAN_POINT('Ctrl Pts',(-0.0949643705016135,0.116711791945748,
0.319999313815503));
#19227=CARTESIAN_POINT('Ctrl Pts',(-0.149558357514911,-0.0164976283567656,
0.327938303452809));
#19228=CARTESIAN_POINT('Ctrl Pts',(-0.0672419181269484,-0.134604600554976,
0.335877293090115));
#19229=CARTESIAN_POINT('Ctrl Pts',(0.0766298889166206,-0.12949028600085,
0.343816282727421));
#19230=CARTESIAN_POINT('Ctrl Pts',(0.150352284446295,-0.00583648916182633,
0.351755272364726));
#19231=CARTESIAN_POINT('Ctrl Pts',(0.0864374678803939,0.123160213504125,
0.359694262002032));
#19232=CARTESIAN_POINT('Ctrl Pts',(-0.0566049265834532,0.139412181427728,
0.367633251639338));
#19233=CARTESIAN_POINT('Ctrl Pts',(-0.147829390149123,0.0280418517950267,
0.375572241276644));
#19234=CARTESIAN_POINT('Ctrl Pts',(-0.103726178443039,-0.108998871322406,
0.383511230913949));
#19235=CARTESIAN_POINT('Ctrl Pts',(0.0353312408083745,-0.146258597924691,
0.391450220551255));
#19236=CARTESIAN_POINT('Ctrl Pts',(0.142045330507792,-0.0496286018832686,
0.399389210188561));
#19237=CARTESIAN_POINT('Ctrl Pts',(0.118726655129599,0.0924329779120693,
0.407328199825866));
#19238=CARTESIAN_POINT('Ctrl Pts',(-0.0132781361506635,0.1498785012746,
0.415267189463172));
#19239=CARTESIAN_POINT('Ctrl Pts',(-0.133127703795094,0.0701205285647604,
0.423206179100478));
#19240=CARTESIAN_POINT('Ctrl Pts',(-0.131107982452518,-0.0738279823724454,
0.431145168737783));
#19241=CARTESIAN_POINT('Ctrl Pts',(-0.00906788859151817,-0.150192035209753,
0.439084158375089));
#19242=CARTESIAN_POINT('Ctrl Pts',(0.121273235812024,-0.0890655731449414,
0.447023148012395));
#19243=CARTESIAN_POINT('Ctrl Pts',(0.14059702422731,0.0535943170716914,
0.4549621376497));
#19244=CARTESIAN_POINT('Ctrl Pts',(0.031213872705855,0.14719228306762,0.462901127287006));
#19245=CARTESIAN_POINT('Ctrl Pts',(-0.106743440051405,0.106045801661112,
0.470840116924312));
#19246=CARTESIAN_POINT('Ctrl Pts',(-0.146984449047318,-0.0321783433727119,
0.478779106561618));
#19247=CARTESIAN_POINT('Ctrl Pts',(-0.0526712684425847,-0.140945420374714,
0.486718096198923));
#19248=CARTESIAN_POINT('Ctrl Pts',(0.0898588486235595,-0.120686624644175,
0.49465708583623));
#19249=CARTESIAN_POINT('Ctrl Pts',(0.150129348203927,0.0100525047535443,
0.502596075473534));
#19250=CARTESIAN_POINT('Ctrl Pts',(0.0729667185397875,0.131589254992538,
0.510535065110842));
#19251=CARTESIAN_POINT('Ctrl Pts',(-0.0709919412117167,0.132665060686482,
0.518474054748145));
#19252=CARTESIAN_POINT('Ctrl Pts',(-0.149962344179375,0.0122950954523496,
0.526413044385453));
#19253=CARTESIAN_POINT('Ctrl Pts',(-0.0916524986414713,-0.119330187030486,
0.534352034022757));
#19254=CARTESIAN_POINT('Ctrl Pts',(0.0505589280467443,-0.141716861518734,
0.542291023660064));
#19255=CARTESIAN_POINT('Ctrl Pts',(0.146487121137799,-0.0343714617774037,
0.550230013297369));
#19256=CARTESIAN_POINT('Ctrl Pts',(0.108316394245265,0.104438655591022,
0.558169002934674));
#19257=CARTESIAN_POINT('Ctrl Pts',(-0.0290105681715044,0.147642341414387,
0.566107992571982));
#19258=CARTESIAN_POINT('Ctrl Pts',(-0.139780343651344,0.0556895822633619,
0.574046982209285));
#19259=CARTESIAN_POINT('Ctrl Pts',(-0.122590794290966,-0.0872431727934394,
0.581985971846593));
#19260=CARTESIAN_POINT('Ctrl Pts',(0.00682222554696161,-0.150310782322966,
0.589924961483898));
#19261=CARTESIAN_POINT('Ctrl Pts',(0.129989965454297,-0.0757791721064987,
0.597863951121203));
#19262=CARTESIAN_POINT('Ctrl Pts',(0.134160800782372,0.0681230766876274,
0.60580294075851));
#19263=CARTESIAN_POINT('Ctrl Pts',(0.015516617634347,0.149663317553585,
0.613741930395814));
#19264=CARTESIAN_POINT('Ctrl Pts',(-0.117331965534667,0.0941970482962578,
0.621680920033121));
#19265=CARTESIAN_POINT('Ctrl Pts',(-0.142771175541451,-0.0475001629309618,
0.629619909670426));
#19266=CARTESIAN_POINT('Ctrl Pts',(-0.0375131590877193,-0.145714230393655,
0.637558899307733));
#19267=CARTESIAN_POINT('Ctrl Pts',(0.102085583566124,-0.110536906379362,
0.645497888945037));
#19268=CARTESIAN_POINT('Ctrl Pts',(0.148231970847143,0.0258293798362968,
0.653436878582344));
#19269=CARTESIAN_POINT('Ctrl Pts',(0.0586821478180281,0.138550639014834,
0.661375868219649));
#19270=CARTESIAN_POINT('Ctrl Pts',(-0.0845871597882484,0.124438283670714,
0.669314857856955));
#19271=CARTESIAN_POINT('Ctrl Pts',(-0.150422719745043,-0.00358879206139753,
0.67725384749426));
#19272=CARTESIAN_POINT('Ctrl Pts',(-0.078556588917505,-0.128330574617282,
0.685192837131567));
#19273=CARTESIAN_POINT('Ctrl Pts',(0.065222715229363,-0.135594511179713,
0.693131826768872));
#19274=CARTESIAN_POINT('Ctrl Pts',(0.149295093588351,-0.0187309656558678,
0.701070816406178));
#19275=CARTESIAN_POINT('Ctrl Pts',(0.0966980456281902,0.11527949520901,
0.709009806043483));
#19276=CARTESIAN_POINT('Ctrl Pts',(-0.044419435954706,0.14375947882982,
0.716948795680789));
#19277=CARTESIAN_POINT('Ctrl Pts',(-0.144873968183829,0.0406375120624596,
0.724887785318095));
#19278=CARTESIAN_POINT('Ctrl Pts',(-0.112706311402131,-0.099685311927494,
0.732826774955401));
#19279=CARTESIAN_POINT('Ctrl Pts',(0.0226362492002416,-0.148753064728429,
0.740765764592706));
#19280=CARTESIAN_POINT('Ctrl Pts',(0.137256875023267,-0.0616475814838108,
0.748704754230013));
#19281=CARTESIAN_POINT('Ctrl Pts',(0.126228238590478,0.0818920376245527,
0.756643743867318));
#19282=CARTESIAN_POINT('Ctrl Pts',(-0.000353699285724532,0.150465108715513,
0.764582733504624));
#19283=CARTESIAN_POINT('Ctrl Pts',(-0.126611849706441,0.0812976848247803,
0.772521723141928));
#19284=CARTESIAN_POINT('Ctrl Pts',(-0.136965528997667,-0.0622921978288208,
0.780460712779236));
#19285=CARTESIAN_POINT('Ctrl Pts',(-0.0219366533522686,-0.148857842533265,
0.788399702416541));
#19286=CARTESIAN_POINT('Ctrl Pts',(0.113173725020093,-0.0991543342927188,
0.796338692053846));
#19287=CARTESIAN_POINT('Ctrl Pts',(0.144681314438483,0.0413181715024817,
0.804277681691154));
#19288=CARTESIAN_POINT('Ctrl Pts',(0.0437430761464933,0.143966723006387,
0.812216671328456));
#19289=CARTESIAN_POINT('Ctrl Pts',(-0.0972389504488157,0.114823606281847,
0.820155660965765));
#19290=CARTESIAN_POINT('Ctrl Pts',(-0.149205382128735,-0.0194326526180533,
0.828094650603069));
#19291=CARTESIAN_POINT('Ctrl Pts',(-0.0645845121824554,-0.135899649852787,
0.836033640240376));
#19292=CARTESIAN_POINT('Ctrl Pts',(0.0791590524011713,-0.127959831458565,
0.843972629877681));
#19293=CARTESIAN_POINT('Ctrl Pts',(0.150437929635691,-0.00288155702400619,
0.851911619514986));
#19294=CARTESIAN_POINT('Ctrl Pts',(0.0840011924733913,0.12483458538003,
0.859850609152293));
#19295=CARTESIAN_POINT('Ctrl Pts',(-0.0593328794206009,0.138273220341526,
0.867789598789597));
#19296=CARTESIAN_POINT('Ctrl Pts',(-0.148351766552825,0.0251321985630355,
0.875728588426904));
#19297=CARTESIAN_POINT('Ctrl Pts',(-0.1015647786165,-0.111015628577859,
0.883667578064211));
#19298=CARTESIAN_POINT('Ctrl Pts',(0.0381978034543637,-0.145536256153639,
0.891606567701514));
#19299=CARTESIAN_POINT('Ctrl Pts',(0.142992914329196,-0.046828415471795,
0.899545557338823));
#19300=CARTESIAN_POINT('Ctrl Pts',(0.116887812080083,0.0947476302135675,
0.907484546976125));
#19301=CARTESIAN_POINT('Ctrl Pts',(-0.0162200712834111,0.149588713917584,
0.915423536613434));
#19302=CARTESIAN_POINT('Ctrl Pts',(-0.134479591021026,0.067491582014154,
0.923362526250738));
#19303=CARTESIAN_POINT('Ctrl Pts',(-0.129632261667175,-0.0763894677230377,
0.931301515888044));
#19304=CARTESIAN_POINT('Ctrl Pts',(-0.00611548103612966,-0.150341195071919,
0.93924050552535));
#19305=CARTESIAN_POINT('Ctrl Pts',(0.122999603362204,-0.0866658618874593,
0.947179495162656));
#19306=CARTESIAN_POINT('Ctrl Pts',(0.139516980595786,0.0563461282555487,
0.95511848479996));
#19307=CARTESIAN_POINT('Ctrl Pts',(0.0283161238170646,0.147777099632969,
0.963057474437267));
#19308=CARTESIAN_POINT('Ctrl Pts',(-0.108806203685475,0.103928264122473,
0.970996464074573));
#19309=CARTESIAN_POINT('Ctrl Pts',(-0.146323908690103,-0.0350597745230392,
0.978935453711877));
#19310=CARTESIAN_POINT('Ctrl Pts',(-0.049892103521326,-0.14195299239598,
0.986874443349185));
#19311=CARTESIAN_POINT('Ctrl Pts',(0.0922125030920605,-0.118897974404329,
0.994813432986488));
#19312=CARTESIAN_POINT('Ctrl Pts',(0.149902882860231,0.0129999905441286,
1.0027524226238));
#19313=CARTESIAN_POINT('Ctrl Pts',(0.0703674468853664,0.132997355096976,
1.0106914122611));
#19314=CARTESIAN_POINT('Ctrl Pts',(-0.0735845641169637,0.131244755962562,
1.01863040189841));
#19315=CARTESIAN_POINT('Ctrl Pts',(-0.150174949749745,0.00934657753497952,
1.02656939153571));
#19316=CARTESIAN_POINT('Ctrl Pts',(-0.0892904610481016,-0.121107752063083,
1.03450838117302));
#19317=CARTESIAN_POINT('Ctrl Pts',(0.0533333252681307,-0.140696234703703,
1.04244737081032));
#19318=CARTESIAN_POINT('Ctrl Pts',(0.147134107472884,-0.031486957015783,
1.05038636044763));
#19319=CARTESIAN_POINT('Ctrl Pts',(0.106243698045146,0.106546471877992,
1.05832535008494));
#19320=CARTESIAN_POINT('Ctrl Pts',(-0.0319055355867657,0.147043907874068,
1.06626433972224));
#19321=CARTESIAN_POINT('Ctrl Pts',(-0.14084743801815,0.0529327237885883,
1.07420332935955));
#19322=CARTESIAN_POINT('Ctrl Pts',(-0.120853163849259,-0.0896347412088629,
1.08214231899685));
#19323=CARTESIAN_POINT('Ctrl Pts',(0.00977389921538986,-0.150147743699608,
1.09008130863416));
#19324=CARTESIAN_POINT('Ctrl Pts',(0.13145362739741,-0.0732107771302755,
1.09802029827146));
#19325=CARTESIAN_POINT('Ctrl Pts',(0.132796568802552,0.0707456384395876,
1.10595928790877));
#19326=CARTESIAN_POINT('Ctrl Pts',(0.0125733526121963,0.149939270533256,
1.11389827754607));
#19327=CARTESIAN_POINT('Ctrl Pts',(-0.119159906186493,0.0918737764630459,
1.12183726718338));
#19328=CARTESIAN_POINT('Ctrl Pts',(-0.141810437433163,-0.0502958634379693,
1.12977625682069));
#19329=CARTESIAN_POINT('Ctrl Pts',(-0.0346432321137694,-0.146423087362162,
1.13771524645799));
#19330=CARTESIAN_POINT('Ctrl Pts',(0.104237477950025,-0.108510009835838,
1.1456542360953));
#19331=CARTESIAN_POINT('Ctrl Pts',(0.147695920811486,0.0287365450185451,
1.1535932257326));
#19332=CARTESIAN_POINT('Ctrl Pts',(0.0559488704325515,0.139676762352502,
1.16153221536991));
#19333=CARTESIAN_POINT('Ctrl Pts',(-0.0870155364008756,0.12275247642644,
1.16947120500722));
#19334=CARTESIAN_POINT('Ctrl Pts',(-0.150323183223479,-0.00654328889139735,
1.17741019464452));
#19335=CARTESIAN_POINT('Ctrl Pts',(-0.0760202581255566,-0.129849121670035,
1.18534918428183));
#19336=CARTESIAN_POINT('Ctrl Pts',(0.0678740032777675,-0.134286982701248,
1.19328817391913));
#19337=CARTESIAN_POINT('Ctrl Pts',(0.149634266389533,-0.0157943143574443,
1.20122716355644));
#19338=CARTESIAN_POINT('Ctrl Pts',(0.0944146137277022,0.117156966325547,
1.20916615319374));
#19339=CARTESIAN_POINT('Ctrl Pts',(-0.047235147145783,0.142859073628774,
1.21710514283105));
#19340=CARTESIAN_POINT('Ctrl Pts',(-0.145644368043342,0.037783489796601,
1.22504413246835));
#19341=CARTESIAN_POINT('Ctrl Pts',(-0.11072615165767,-0.101880289472715,
1.23298312210566));
#19342=CARTESIAN_POINT('Ctrl Pts',(0.0255542680118797,-0.148279646041953,
1.24092211174296));
#19343=CARTESIAN_POINT('Ctrl Pts',(0.138441506664824,-0.0589391489276913,
1.24886110138027));
#19344=CARTESIAN_POINT('Ctrl Pts',(0.124595033982396,0.0843560996663564,
1.25680009101758));
#19345=CARTESIAN_POINT('Ctrl Pts',(-0.00330965325590636,0.150429120316621,
1.26473908065488));
#19346=CARTESIAN_POINT('Ctrl Pts',(-0.128184579763139,0.0787945908985174,
1.27267807029219));
#19347=CARTESIAN_POINT('Ctrl Pts',(-0.135715308561414,-0.0649709863423027,
1.2806170599295));
#19348=CARTESIAN_POINT('Ctrl Pts',(-0.0190079735469551,-0.149260078337129,
1.2885560495668));
#19349=CARTESIAN_POINT('Ctrl Pts',(0.115099858543875,-0.0969117980795561,
1.29649503920411));
#19350=CARTESIAN_POINT('Ctrl Pts',(0.143841658454547,0.0441525915281748,
1.30443402884141));
#19351=CARTESIAN_POINT('Ctrl Pts',(0.0409062781470196,0.144798309552134,
1.31237301847872));
#19352=CARTESIAN_POINT('Ctrl Pts',(-0.0994759962839106,0.112891098884786,
1.32031200811602));
#19353=CARTESIAN_POINT('Ctrl Pts',(-0.148794813708878,-0.0223601759313527,
1.32825099775333));
#19354=CARTESIAN_POINT('Ctrl Pts',(-0.0619021766503053,-0.13714224202644,
1.33618998739064));
#19355=CARTESIAN_POINT('Ctrl Pts',(0.0816576604940555,-0.126379984705639,
1.34412897702794));
#19356=CARTESIAN_POINT('Ctrl Pts',(0.150465506209006,7.4487583413377E-5,
1.35206796666525));
#19357=CARTESIAN_POINT('Ctrl Pts',(0.0815324923277053,0.126460770918471,
1.36000695630255));
#19358=CARTESIAN_POINT('Ctrl Pts',(-0.062037929094705,0.137080886684378,
1.36794594593986));
#19359=CARTESIAN_POINT('Ctrl Pts',(-0.148816880822527,0.0222128430196456,
1.37588493557716));
#19360=CARTESIAN_POINT('Ctrl Pts',(-0.0993641722043223,-0.112989531455785,
1.38382392521447));
#19361=CARTESIAN_POINT('Ctrl Pts',(0.0410496166270677,-0.144757742348562,
1.39176291485178));
#19362=CARTESIAN_POINT('Ctrl Pts',(0.143885312916173,-0.0440101443352923,
1.39970190448908));
#19363=CARTESIAN_POINT('Ctrl Pts',(0.115003831846793,0.0970256929337524,
1.40764089412639));
#19364=CARTESIAN_POINT('Ctrl Pts',(-0.0191557100743377,0.149241218055048,
1.41557988376369));
#19365=CARTESIAN_POINT('Ctrl Pts',(-0.135779636557791,0.0648365220611291,
1.423518873401));
#19366=CARTESIAN_POINT('Ctrl Pts',(-0.128106375355825,-0.0789213496179777,
1.4314578630383));
#19367=CARTESIAN_POINT('Ctrl Pts',(-0.00316095527563228,-0.150432546011701,
1.43939685267561));
#19368=CARTESIAN_POINT('Ctrl Pts',(0.12467895337041,-0.0842322751882648,
1.44733584231291));
#19369=CARTESIAN_POINT('Ctrl Pts',(0.138382210043398,0.0590753877074232,
1.45527483195022));
#19370=CARTESIAN_POINT('Ctrl Pts',(0.0254091034322018,0.148306397458819,
1.46321382158753));
#19371=CARTESIAN_POINT('Ctrl Pts',(-0.110830116988615,0.101767718932792,
1.47115281122483));
#19372=CARTESIAN_POINT('Ctrl Pts',(-0.145600909330124,-0.0379221829034233,
1.47909180086214));
#19373=CARTESIAN_POINT('Ctrl Pts',(-0.0471050325108872,-0.142916194795756,
1.48703079049945));
#19374=CARTESIAN_POINT('Ctrl Pts',(0.0945521370959566,-0.117043625665234,
1.49496978013675));
#19375=CARTESIAN_POINT('Ctrl Pts',(0.14957741911039,0.0159047428854941,
1.50290876977406));
#19376=CARTESIAN_POINT('Ctrl Pts',(0.0678206238522695,0.134426714629862,
1.51084775941136));
#19377=CARTESIAN_POINT('Ctrl Pts',(-0.0763126473618499,0.129627546381738,
1.51878674904867));
#19378=CARTESIAN_POINT('Ctrl Pts',(-0.125385920115907,0.0477050348167321,
1.52407940880687));
#19379=CARTESIAN_POINT('Ctrl Pts',(-0.127184992207234,0.00540996832206346,
1.52672573868597));
#19380=CARTESIAN_POINT('Ctrl Pts',(0.0684664424539414,-0.095829519891843,
-1.38777878078145E-17));
#19381=CARTESIAN_POINT('Ctrl Pts',(0.100334321247169,-0.0730611673843044,
0.00264632987910189));
#19382=CARTESIAN_POINT('Ctrl Pts',(0.139021564822767,0.00636891437108143,
0.00793898963730573));
#19383=CARTESIAN_POINT('Ctrl Pts',(0.0699018669780613,0.120491966796142,
0.0158779792746114));
#19384=CARTESIAN_POINT('Ctrl Pts',(-0.0632645460347191,0.123954346655885,
0.0238169689119172));
#19385=CARTESIAN_POINT('Ctrl Pts',(-0.138486976988987,0.0141253725679007,
0.0317559585492228));
#19386=CARTESIAN_POINT('Ctrl Pts',(-0.0869496735326521,-0.108728403071097,
0.0396949481865287));
#19387=CARTESIAN_POINT('Ctrl Pts',(0.0441923146003338,-0.131999388615902,
0.0476339378238343));
#19388=CARTESIAN_POINT('Ctrl Pts',(0.134874939024977,-0.034459980695041,
0.0555729274611401));
#19389=CARTESIAN_POINT('Ctrl Pts',(0.102091080224759,0.094638871230671,
0.0635119170984456));
#19390=CARTESIAN_POINT('Ctrl Pts',(-0.0241513666277066,0.137095110112719,
0.0714509067357516));
#19391=CARTESIAN_POINT('Ctrl Pts',(-0.128284260007319,0.0540539703915629,
0.0793898963730571));
#19392=CARTESIAN_POINT('Ctrl Pts',(-0.114982038412656,-0.0784718756714057,
0.0873288860103631));
#19393=CARTESIAN_POINT('Ctrl Pts',(0.00357853460314598,-0.139161043603659,
0.0952678756476685));
#19394=CARTESIAN_POINT('Ctrl Pts',(0.118863112008681,-0.0724583686054966,
0.103206865284975));
#19395=CARTESIAN_POINT('Ctrl Pts',(0.125336705278751,0.0605752693714656,
0.11114585492228));
#19396=CARTESIAN_POINT('Ctrl Pts',(0.0170731091066207,0.138156245709763,
0.119084844559586));
#19397=CARTESIAN_POINT('Ctrl Pts',(-0.106819734848208,0.0892647286947484,
0.127023834196891));
#19398=CARTESIAN_POINT('Ctrl Pts',(-0.132926439498961,-0.0413425724611633,
0.134962823834197));
#19399=CARTESIAN_POINT('Ctrl Pts',(-0.0373480950846616,-0.134103559412242,
0.142901813471503));
#19400=CARTESIAN_POINT('Ctrl Pts',(0.0924198687735613,-0.104101940294199,
0.150840803108809));
#19401=CARTESIAN_POINT('Ctrl Pts',(0.137583777756591,0.0211978768359354,
0.158779792746114));
#19402=CARTESIAN_POINT('Ctrl Pts',(0.0567991668878991,0.127092487218924,
0.16671878238342));
#19403=CARTESIAN_POINT('Ctrl Pts',(-0.075981188277068,0.116642637502503,
0.174657772020726));
#19404=CARTESIAN_POINT('Ctrl Pts',(-0.139205973057234,-0.000585553717998882,
0.182596761658032));
#19405=CARTESIAN_POINT('Ctrl Pts',(-0.0749972298318695,-0.11727771015962,
0.190535751295337));
#19406=CARTESIAN_POINT('Ctrl Pts',(0.0578663373665801,-0.126610160769685,
0.198474740932643));
#19407=CARTESIAN_POINT('Ctrl Pts',(0.13775723856723,-0.0200396862227523,
0.206413730569949));
#19408=CARTESIAN_POINT('Ctrl Pts',(0.091540828968026,0.104875747581476,
0.214352720207254));
#19409=CARTESIAN_POINT('Ctrl Pts',(-0.0384749358425138,0.133784622116252,
0.22229170984456));
#19410=CARTESIAN_POINT('Ctrl Pts',(-0.133269533752038,0.0402228439430644,
0.230230699481866));
#19411=CARTESIAN_POINT('Ctrl Pts',(-0.106065007067505,-0.0901601911982067,
0.238169689119172));
#19412=CARTESIAN_POINT('Ctrl Pts',(0.0182347644767634,-0.138007750384372,
0.246108678756477));
#19413=CARTESIAN_POINT('Ctrl Pts',(0.125841858853055,-0.0595186723796334,
0.254047668393783));
#19414=CARTESIAN_POINT('Ctrl Pts',(0.118249355954961,0.073455671106145,
0.261986658031089));
#19415=CARTESIAN_POINT('Ctrl Pts',(0.00240767183786234,0.139186381940956,
0.269925647668394));
#19416=CARTESIAN_POINT('Ctrl Pts',(-0.115638070838342,0.0775014991741366,
0.277864637305701));
#19417=CARTESIAN_POINT('Ctrl Pts',(-0.12782508485658,-0.0551306945617612,
0.285803626943006));
#19418=CARTESIAN_POINT('Ctrl Pts',(-0.0229969941138309,-0.137294515779738,
0.293742616580312));
#19419=CARTESIAN_POINT('Ctrl Pts',(0.102883268653204,-0.0937746172089793,
0.301681606217617));
#19420=CARTESIAN_POINT('Ctrl Pts',(0.134580950019115,0.0355895166223291,
0.309620595854923));
#19421=CARTESIAN_POINT('Ctrl Pts',(0.0430789950773988,0.13237388709478,
0.317559585492229));
#19422=CARTESIAN_POINT('Ctrl Pts',(-0.0878588274613298,0.107979036106918,
0.325498575129534));
#19423=CARTESIAN_POINT('Ctrl Pts',(-0.1383679148179,-0.0152632221501787,
0.33343756476684));
#19424=CARTESIAN_POINT('Ctrl Pts',(-0.0622106591311991,-0.12453304658572,
0.341376554404146));
#19425=CARTESIAN_POINT('Ctrl Pts',(0.0708961914151981,-0.119801401679107,
0.349315544041452));
#19426=CARTESIAN_POINT('Ctrl Pts',(0.1391024375543,-0.00539978406154301,
0.357254533678757));
#19427=CARTESIAN_POINT('Ctrl Pts',(0.0799699354250877,0.113944965792994,
0.365193523316063));
#19428=CARTESIAN_POINT('Ctrl Pts',(-0.0523695618881846,0.128980908622551,
0.373132512953369));
#19429=CARTESIAN_POINT('Ctrl Pts',(-0.136768314413298,0.0259436692471295,
0.381071502590675));
#19430=CARTESIAN_POINT('Ctrl Pts',(-0.0959650484377783,-0.100843221288265,
0.38901049222798));
#19431=CARTESIAN_POINT('Ctrl Pts',(0.0326876424682324,-0.135315053971568,
0.396949481865287));
#19432=CARTESIAN_POINT('Ctrl Pts',(0.13141703692502,-0.0459152284901983,
0.404888471502591));
#19433=CARTESIAN_POINT('Ctrl Pts',(0.109843140674695,0.0855168418978295,
0.412827461139898));
#19434=CARTESIAN_POINT('Ctrl Pts',(-0.0122846228212416,0.13866410438033,
0.420766450777203));
#19435=CARTESIAN_POINT('Ctrl Pts',(-0.123166656044517,0.0648738825743514,
0.428705440414509));
#19436=CARTESIAN_POINT('Ctrl Pts',(-0.121298056821252,-0.0683039326309071,
0.436644430051815));
#19437=CARTESIAN_POINT('Ctrl Pts',(-0.00838939967687663,-0.138954178686792,
0.44458341968912));
#19438=CARTESIAN_POINT('Ctrl Pts',(0.11219917790857,-0.0824013973067221,
0.452522409326426));
#19439=CARTESIAN_POINT('Ctrl Pts',(0.13007709763057,0.0495842159710775,
0.460461398963732));
#19440=CARTESIAN_POINT('Ctrl Pts',(0.0288783492374893,0.136178877755608,
0.468400388601037));
#19441=CARTESIAN_POINT('Ctrl Pts',(-0.0987565487199846,0.0981111099028881,
0.476339378238344));
#19442=CARTESIAN_POINT('Ctrl Pts',(-0.135986594552616,-0.0297706550724338,
0.484278367875649));
#19443=CARTESIAN_POINT('Ctrl Pts',(-0.0487302328423073,-0.130399425645183,
0.492217357512954));
#19444=CARTESIAN_POINT('Ctrl Pts',(0.0831353173341669,-0.111656458896056,
0.50015634715026));
#19445=CARTESIAN_POINT('Ctrl Pts',(0.13889618212661,0.00930034365552528,
0.508095336787567));
#19446=CARTESIAN_POINT('Ctrl Pts',(0.0675071113591811,0.12174331898465,
0.516034326424871));
#19447=CARTESIAN_POINT('Ctrl Pts',(-0.0656800932930844,0.122738629397884,
0.523973316062178));
#19448=CARTESIAN_POINT('Ctrl Pts',(-0.138741673886299,0.0113751364249866,
0.531912305699483));
#19449=CARTESIAN_POINT('Ctrl Pts',(-0.0847947606245053,-0.110401514355972,
0.539851295336789));
#19450=CARTESIAN_POINT('Ctrl Pts',(0.0467759446245483,-0.131113145053959,
0.547790284974095));
#19451=CARTESIAN_POINT('Ctrl Pts',(0.135526478334676,-0.031799677225719,
0.555729274611401));
#19452=CARTESIAN_POINT('Ctrl Pts',(0.100211809365564,0.0966242157284558,
0.563668264248707));
#19453=CARTESIAN_POINT('Ctrl Pts',(-0.0268399031138932,0.136595261273209,
0.571607253886012));
#19454=CARTESIAN_POINT('Ctrl Pts',(-0.129321523751272,0.0515227066069736,
0.579546243523318));
#19455=CARTESIAN_POINT('Ctrl Pts',(-0.113418152377209,-0.0807153548762533,
0.587485233160623));
#19456=CARTESIAN_POINT('Ctrl Pts',(0.00631176444456456,-0.139064040754811,
0.595424222797929));
#19457=CARTESIAN_POINT('Ctrl Pts',(0.120263693490807,-0.0701091280034811,
0.603363212435234));
#19458=CARTESIAN_POINT('Ctrl Pts',(0.124122453355413,0.0630258865426945,
0.611302202072541));
#19459=CARTESIAN_POINT('Ctrl Pts',(0.0143556138404206,0.138465021405133,
0.619241191709845));
#19460=CARTESIAN_POINT('Ctrl Pts',(-0.108552806291007,0.0871489187988374,
0.627180181347153));
#19461=CARTESIAN_POINT('Ctrl Pts',(-0.132088571872698,-0.043946046262323,
0.635119170984457));
#19462=CARTESIAN_POINT('Ctrl Pts',(-0.0347063025259737,-0.134811417789573,
0.643058160621763));
#19463=CARTESIAN_POINT('Ctrl Pts',(0.0944472082050275,-0.102266175560326,
0.65099715025907));
#19464=CARTESIAN_POINT('Ctrl Pts',(0.137140772714236,0.0238967416356601,
0.658936139896373));
#19465=CARTESIAN_POINT('Ctrl Pts',(0.054291358674537,0.128183829614862,
0.666875129533682));
#19466=CARTESIAN_POINT('Ctrl Pts',(-0.0782580734018908,0.115127406593233,
0.674814119170985));
#19467=CARTESIAN_POINT('Ctrl Pts',(-0.139167602654929,-0.00332026696803425,
0.682753108808293));
#19468=CARTESIAN_POINT('Ctrl Pts',(-0.0726787294560835,-0.118728463672822,
0.690692098445597));
#19469=CARTESIAN_POINT('Ctrl Pts',(0.0603425395611779,-0.125448888878168,
0.698631088082904));
#19470=CARTESIAN_POINT('Ctrl Pts',(0.138124349154501,-0.0173294538893964,
0.706570077720209));
#19471=CARTESIAN_POINT('Ctrl Pts',(0.0894627833767505,0.106653908470079,
0.714509067357515));
#19472=CARTESIAN_POINT('Ctrl Pts',(-0.0410958292974484,0.133002927094911,
0.72244805699482));
#19473=CARTESIAN_POINT('Ctrl Pts',(-0.134034026730954,0.0375968812502473,
0.730387046632127));
#19474=CARTESIAN_POINT('Ctrl Pts',(-0.104273258644039,-0.0922265326964679,
0.738326036269432));
#19475=CARTESIAN_POINT('Ctrl Pts',(0.0209425314183671,-0.137622876656644,
0.746265025906738));
#19476=CARTESIAN_POINT('Ctrl Pts',(0.126986869252672,-0.0570349089493802,
0.754204015544043));
#19477=CARTESIAN_POINT('Ctrl Pts',(0.11678343126468,0.0757646090434518,
0.762143005181349));
#19478=CARTESIAN_POINT('Ctrl Pts',(-0.000327234354877375,0.139206819944772,
0.770081994818654));
#19479=CARTESIAN_POINT('Ctrl Pts',(-0.117138339349379,0.0752147276530931,
0.778020984455961));
#19480=CARTESIAN_POINT('Ctrl Pts',(-0.126717322684213,-0.0576312930030564,
0.785959974093266));
#19481=CARTESIAN_POINT('Ctrl Pts',(-0.0202952816069424,-0.137719814645367,
0.793898963730571));
#19482=CARTESIAN_POINT('Ctrl Pts',(0.104705698854998,-0.0917352845351548,
0.801837953367879));
#19483=CARTESIAN_POINT('Ctrl Pts',(0.133855787965376,0.0382266115373486,
0.809776943005182));
#19484=CARTESIAN_POINT('Ctrl Pts',(0.0404700769297216,0.133194664588195,
0.81771593264249));
#19485=CARTESIAN_POINT('Ctrl Pts',(-0.0899632159395838,0.106232130635072,
0.825654922279794));
#19486=CARTESIAN_POINT('Ctrl Pts',(-0.13804135019805,-0.0179786383510676,
0.833593911917101));
#19487=CARTESIAN_POINT('Ctrl Pts',(-0.059752088941783,-0.125731196083361,
0.841532901554406));
#19488=CARTESIAN_POINT('Ctrl Pts',(0.0732361146625898,-0.118385460722959,
0.849471891191712));
#19489=CARTESIAN_POINT('Ctrl Pts',(0.139181674492094,-0.00266594955618734,
0.857410880829018));
#19490=CARTESIAN_POINT('Ctrl Pts',(0.077715950067195,0.115494055719818,
0.865349870466323));
#19491=CARTESIAN_POINT('Ctrl Pts',(-0.0548934004223171,0.127927168308903,
0.87328886010363));
#19492=CARTESIAN_POINT('Ctrl Pts',(-0.137251604915624,0.0232517257326144,
0.881227849740934));
#19493=CARTESIAN_POINT('Ctrl Pts',(-0.0939653715754795,-0.102709078207047,
0.889166839378241));
#19494=CARTESIAN_POINT('Ctrl Pts',(0.0353397195745277,-0.134646760160997,
0.897105829015547));
#19495=CARTESIAN_POINT('Ctrl Pts',(0.132293719443212,-0.0433245611326863,
0.905044818652852));
#19496=CARTESIAN_POINT('Ctrl Pts',(0.108141885842356,0.0876583043865096,
0.912983808290157));
#19497=CARTESIAN_POINT('Ctrl Pts',(-0.0150064327997127,0.138395999855801,
0.920922797927463));
#19498=CARTESIAN_POINT('Ctrl Pts',(-0.124417390671652,0.0624416423544169,
0.928861787564769));
#19499=CARTESIAN_POINT('Ctrl Pts',(-0.119932754264349,-0.0706737593172073,
0.936800777202075));
#19500=CARTESIAN_POINT('Ctrl Pts',(-0.00565790085648466,-0.139092177922979,
0.944739766839381));
#19501=CARTESIAN_POINT('Ctrl Pts',(0.113796373024222,-0.0801812402497705,
0.952678756476687));
#19502=CARTESIAN_POINT('Ctrl Pts',(0.129077866376032,0.0521301276928276,
0.960617746113992));
#19503=CARTESIAN_POINT('Ctrl Pts',(0.026197419344502,0.13671993644362,0.968556735751298));
#19504=CARTESIAN_POINT('Ctrl Pts',(-0.100664969670515,0.0961520134094621,
0.976495725388603));
#19505=CARTESIAN_POINT('Ctrl Pts',(-0.13537547797311,-0.0324364881732178,
0.98443471502591));
#19506=CARTESIAN_POINT('Ctrl Pts',(-0.0461590140787468,-0.131331607851033,
0.992373704663214));
#19507=CARTESIAN_POINT('Ctrl Pts',(0.0853128637208732,-0.110001641284132,
1.00031269430052));
#19508=CARTESIAN_POINT('Ctrl Pts',(0.138686661656432,0.0120272889735618,
1.00825168393783));
#19509=CARTESIAN_POINT('Ctrl Pts',(0.0651023256631918,0.123046060459907,
1.01619067357513));
#19510=CARTESIAN_POINT('Ctrl Pts',(-0.0680787277209358,0.121424596492465,
1.02412966321244));
#19511=CARTESIAN_POINT('Ctrl Pts',(-0.138938371616466,0.00864723620724691,
1.03206865284975));
#19512=CARTESIAN_POINT('Ctrl Pts',(-0.0826094583655966,-0.112046076191904,
1.04000764248705));
#19513=CARTESIAN_POINT('Ctrl Pts',(0.0493427524230464,-0.130168884856471,
1.04794663212436));
#19514=CARTESIAN_POINT('Ctrl Pts',(0.136125055048066,-0.0291310004912345,
1.05588562176166));
#19515=CARTESIAN_POINT('Ctrl Pts',(0.0982941990358779,0.0985743183458784,
1.06382461139897));
#19516=CARTESIAN_POINT('Ctrl Pts',(-0.0295182596522469,0.136041604476578,
1.07176360103627));
#19517=CARTESIAN_POINT('Ctrl Pts',(-0.130308774647192,0.0489721252490281,
1.07970259067358));
#19518=CARTESIAN_POINT('Ctrl Pts',(-0.111810537096203,-0.0829279783650712,
1.08764158031088));
#19519=CARTESIAN_POINT('Ctrl Pts',(0.00904258428980543,-0.13891320121148,
1.09558056994819));
#19520=CARTESIAN_POINT('Ctrl Pts',(0.121617839487272,-0.067732908692211,
1.1035195595855));
#19521=CARTESIAN_POINT('Ctrl Pts',(0.122860297649024,0.0654522196953821,
1.1114585492228));
#19522=CARTESIAN_POINT('Ctrl Pts',(0.0116325734791967,0.138720326685422,
1.11939753886011));
#19523=CARTESIAN_POINT('Ctrl Pts',(-0.110243974478508,0.0849994817198388,
1.12733652849741));
#19524=CARTESIAN_POINT('Ctrl Pts',(-0.131199719314147,-0.0465325633653302,
1.13527551813472));
#19525=CARTESIAN_POINT('Ctrl Pts',(-0.0320511128216771,-0.13546723577438,
1.14321450777202));
#19526=CARTESIAN_POINT('Ctrl Pts',(0.0964380908528195,-0.100390938007982,
1.15115349740933));
#19527=CARTESIAN_POINT('Ctrl Pts',(0.136644831685568,0.0265863832644056,
1.15909248704664));
#19528=CARTESIAN_POINT('Ctrl Pts',(0.0517625939920979,0.129225692742072,
1.16703147668394));
#19529=CARTESIAN_POINT('Ctrl Pts',(-0.0805047509788913,0.113567736929491,
1.17497046632125));
#19530=CARTESIAN_POINT('Ctrl Pts',(-0.139075513779617,-0.00605369873671642,
1.18290945595855));
#19531=CARTESIAN_POINT('Ctrl Pts',(-0.0703321751825429,-0.12013338809653,
1.19084844559586));
#19532=CARTESIAN_POINT('Ctrl Pts',(0.0627954496153871,-0.124239193932754,
1.19878743523316));
#19533=CARTESIAN_POINT('Ctrl Pts',(0.138438143943654,-0.0146125323915816,
1.20672642487047));
#19534=CARTESIAN_POINT('Ctrl Pts',(0.0873502052771435,0.108390901091839,
1.21466541450777));
#19535=CARTESIAN_POINT('Ctrl Pts',(-0.043700859820065,0.132169893139269,
1.22260440414508));
#19536=CARTESIAN_POINT('Ctrl Pts',(-0.134746782767514,0.0349564062120582,
1.23054339378239));
#19537=CARTESIAN_POINT('Ctrl Pts',(-0.102441260891455,-0.0942572748833364,
1.23848238341969));
#19538=CARTESIAN_POINT('Ctrl Pts',(0.0236422145726536,-0.137184880695923,
1.246421373057));
#19539=CARTESIAN_POINT('Ctrl Pts',(0.128082862902196,-0.0545291301253663,
1.2543603626943));
#19540=CARTESIAN_POINT('Ctrl Pts',(0.115272428336817,0.0780443019497631,
1.26229935233161));
#19541=CARTESIAN_POINT('Ctrl Pts',(-0.00306201423577413,0.139173524314926,
1.27023834196891));
#19542=CARTESIAN_POINT('Ctrl Pts',(-0.118593392628464,0.0728989233548558,
1.27817733160622));
#19543=CARTESIAN_POINT('Ctrl Pts',(-0.125560647806918,-0.06010964584811,
1.28611632124353));
#19544=CARTESIAN_POINT('Ctrl Pts',(-0.0175857351491984,-0.138091953858251,
1.29405531088083));
#19545=CARTESIAN_POINT('Ctrl Pts',(0.106487712804436,-0.089660542174548,
1.30199430051814));
#19546=CARTESIAN_POINT('Ctrl Pts',(0.133078957772855,0.0408489510387311,
1.30993329015544));
#19547=CARTESIAN_POINT('Ctrl Pts',(0.0378455373822902,0.133964029124136,
1.31787227979275));
#19548=CARTESIAN_POINT('Ctrl Pts',(-0.0920328787300654,0.104444219726284,
1.32581126943006));
#19549=CARTESIAN_POINT('Ctrl Pts',(-0.137661501842601,-0.0206871148492911,
1.33375025906736));
#19550=CARTESIAN_POINT('Ctrl Pts',(-0.0572704544775333,-0.126880813469472,
1.34168924870467));
#19551=CARTESIAN_POINT('Ctrl Pts',(0.0755477687720905,-0.116923823242002,
1.34962823834197));
#19552=CARTESIAN_POINT('Ctrl Pts',(0.13920718769651,6.89141801743488E-5,
1.35756722797928));
#19553=CARTESIAN_POINT('Ctrl Pts',(0.0754319660950179,0.116998564767658,
1.36550621761658));
#19554=CARTESIAN_POINT('Ctrl Pts',(-0.0573960494825499,0.126824048933643,
1.37344520725389));
#19555=CARTESIAN_POINT('Ctrl Pts',(-0.13768191782304,0.0205508058651932,
1.38138419689119));
#19556=CARTESIAN_POINT('Ctrl Pts',(-0.0919294216917856,-0.104535287252199,
1.3893231865285));
#19557=CARTESIAN_POINT('Ctrl Pts',(0.0379781508110965,-0.133926497290667,
1.39726217616581));
#19558=CARTESIAN_POINT('Ctrl Pts',(0.133119345865688,-0.0407171622080862,
1.40520116580311));
#19559=CARTESIAN_POINT('Ctrl Pts',(0.106398871137127,0.0897659150453452,
1.41314015544042));
#19560=CARTESIAN_POINT('Ctrl Pts',(-0.0177224175491345,0.138074504763813,
1.42107914507772));
#19561=CARTESIAN_POINT('Ctrl Pts',(-0.125620162573399,0.0599852426217579,
1.42901813471503));
#19562=CARTESIAN_POINT('Ctrl Pts',(-0.118521039729242,-0.0730161975746823,
1.43695712435233));
#19563=CARTESIAN_POINT('Ctrl Pts',(-0.00292444232197888,-0.139176693688359,
1.44489611398964));
#19564=CARTESIAN_POINT('Ctrl Pts',(0.115350068603298,-0.0779297424218237,
1.45283510362695));
#19565=CARTESIAN_POINT('Ctrl Pts',(0.128028003046829,0.0546551750765237,
1.46077409326425));
#19566=CARTESIAN_POINT('Ctrl Pts',(0.0235079116789307,0.137209630484779,
1.46871308290156));
#19567=CARTESIAN_POINT('Ctrl Pts',(-0.102537447198224,0.0941531272373115,
1.47665207253886));
#19568=CARTESIAN_POINT('Ctrl Pts',(-0.134706575776555,-0.0350847218495708,
1.48459106217617));
#19569=CARTESIAN_POINT('Ctrl Pts',(-0.0435804807853106,-0.132222740314769,
1.49253005181348));
#19570=CARTESIAN_POINT('Ctrl Pts',(0.0874774386997331,-0.108286040948335,
1.50046904145078));
#19571=CARTESIAN_POINT('Ctrl Pts',(0.138385550162814,0.0147146982980264,
1.50840803108809));
#19572=CARTESIAN_POINT('Ctrl Pts',(0.0627460642121078,0.124368470664037,
1.51634702072539));
#19573=CARTESIAN_POINT('Ctrl Pts',(-0.0706026869052757,0.119928391791904,
1.5242860103627));
#19574=CARTESIAN_POINT('Ctrl Pts',(-0.116004137797729,0.0441355889673283,
1.5295786701209));
#19575=CARTESIAN_POINT('Ctrl Pts',(-0.117668597464313,0.00500517689812487,
1.532225));
#19576=CARTESIAN_POINT('',(0.0684664424539461,-0.0958295198918396,0.));
#19577=CARTESIAN_POINT('Ctrl Pts',(0.0684664424539414,-0.095829519891843,
-1.38777878078145E-17));
#19578=CARTESIAN_POINT('Ctrl Pts',(0.100334321247169,-0.0730611673843044,
0.00264632987910189));
#19579=CARTESIAN_POINT('Ctrl Pts',(0.139021564822767,0.00636891437108143,
0.00793898963730573));
#19580=CARTESIAN_POINT('Ctrl Pts',(0.0699018669780613,0.120491966796142,
0.0158779792746114));
#19581=CARTESIAN_POINT('Ctrl Pts',(-0.0632645460347191,0.123954346655885,
0.0238169689119172));
#19582=CARTESIAN_POINT('Ctrl Pts',(-0.11596266760442,0.0470121293552651,
0.0293787386625077));
#19583=CARTESIAN_POINT('Ctrl Pts',(-0.117944740497024,0.00404481602818191,
0.0322941785339964));
#19584=CARTESIAN_POINT('Ctrl Pts',(-0.117917485785546,7.60014832213644E-5,
0.0325632885263832));
#19585=CARTESIAN_POINT('Ctrl Pts',(0.0635546915223951,0.132092229195826,
-2.16840434497101E-19));
#19586=CARTESIAN_POINT('Ctrl Pts',(0.0668114782730532,0.13015255741457,
-1.00603861447787E-18));
#19587=CARTESIAN_POINT('Ctrl Pts',(0.0699821360194518,0.12808121947321,
-2.9262196004085E-17));
#19588=CARTESIAN_POINT('Ctrl Pts',(0.0730575207853233,0.125877721325919,
-2.71050543121376E-17));
#19589=CARTESIAN_POINT('Ctrl Pts',(0.0789281193465506,0.121671466161783,
-2.36378102375718E-17));
#19590=CARTESIAN_POINT('Ctrl Pts',(0.0844522091809674,0.11698398814956,
1.43782932504085E-18));
#19591=CARTESIAN_POINT('Ctrl Pts',(0.0895990070394484,0.111875963994554,
9.97465998686664E-18));
#19592=CARTESIAN_POINT('Ctrl Pts',(0.0928865546640729,0.108613183302742,
1.54276111490851E-17));
#19593=CARTESIAN_POINT('Ctrl Pts',(0.0960206821069302,0.105176950779614,
-2.53636710091701E-17));
#19594=CARTESIAN_POINT('Ctrl Pts',(0.098978417360439,0.101599719103904,
-1.56125112837913E-17));
#19595=CARTESIAN_POINT('Ctrl Pts',(0.103148772110026,0.0965558852815647,
-1.86354736740503E-18));
#19596=CARTESIAN_POINT('Ctrl Pts',(0.106976174326278,0.0912251680483688,
1.1337629845105E-17));
#19597=CARTESIAN_POINT('Ctrl Pts',(0.110435561611279,0.0856523061447448,
2.03830008427275E-17));
#19598=CARTESIAN_POINT('Ctrl Pts',(0.112407683932559,0.0824753373788608,
2.55395723911076E-17));
#19599=CARTESIAN_POINT('Ctrl Pts',(0.114261188142284,0.0792174064057451,
2.29308760465575E-17));
#19600=CARTESIAN_POINT('Ctrl Pts',(0.115986535786665,0.0758936579718971,
2.08166817117217E-17));
#19601=CARTESIAN_POINT('Ctrl Pts',(0.120573220307724,0.0670577659456877,
1.51962825639422E-17));
#19602=CARTESIAN_POINT('Ctrl Pts',(0.124235263225439,0.0578042025119142,
2.52358375750583E-18));
#19603=CARTESIAN_POINT('Ctrl Pts',(0.126883306113679,0.0482911783993335,
1.30104260698261E-17));
#19604=CARTESIAN_POINT('Ctrl Pts',(0.128478610866444,0.0425600882242624,
1.93281898253259E-17));
#19605=CARTESIAN_POINT('Ctrl Pts',(0.129704960854084,0.0367345196138549,
-5.78096029915021E-19));
#19606=CARTESIAN_POINT('Ctrl Pts',(0.130533291754837,0.0308494671050701,
0.));
#19607=CARTESIAN_POINT('Ctrl Pts',(0.131003715791213,0.0275072397983871,
3.2831114661813E-19));
#19608=CARTESIAN_POINT('Ctrl Pts',(0.131345346899704,0.0241444941465381,
-1.7128612844445E-18));
#19609=CARTESIAN_POINT('Ctrl Pts',(0.131551728167405,0.0207857616715298,
2.60208521396521E-18));
#19610=CARTESIAN_POINT('Ctrl Pts',(0.131851321606701,0.0159100565018035,
8.86587880453295E-18));
#19611=CARTESIAN_POINT('Ctrl Pts',(0.131867617692795,0.0110341713389591,
-1.68111772803455E-17));
#19612=CARTESIAN_POINT('Ctrl Pts',(0.131586936334964,0.0061777758930637,
-6.93889390390723E-18));
#19613=CARTESIAN_POINT('Ctrl Pts',(0.131099036368572,-0.00226395031615145,
9.98510028643051E-18));
#19614=CARTESIAN_POINT('Ctrl Pts',(0.129715139118287,-0.0106479390144509,
1.03491660509995E-17));
#19615=CARTESIAN_POINT('Ctrl Pts',(0.127493709984164,-0.018859987399606,
1.04083408558608E-17));
#19616=CARTESIAN_POINT('Ctrl Pts',(0.126553994220251,-0.0223338732882013,
1.04333731632617E-17));
#19617=CARTESIAN_POINT('Ctrl Pts',(0.125463061762623,-0.0257782540966497,
1.75224609115742E-17));
#19618=CARTESIAN_POINT('Ctrl Pts',(0.124232565886791,-0.0291638780753137,
1.73472347597681E-17));
#19619=CARTESIAN_POINT('Ctrl Pts',(0.12170396813588,-0.0361211392462112,
1.69871551674183E-17));
#19620=CARTESIAN_POINT('Ctrl Pts',(0.118582485980247,-0.0428512226170345,
-6.45748389186585E-19));
#19621=CARTESIAN_POINT('Ctrl Pts',(0.114911168983798,-0.0492778939609075,
3.46944695195361E-18));
#19622=CARTESIAN_POINT('Ctrl Pts',(0.112347970921096,-0.0537647937721124,
6.34254691478841E-18));
#19623=CARTESIAN_POINT('Ctrl Pts',(0.109516356061708,-0.0581036184196785,
-1.05628593522785E-17));
#19624=CARTESIAN_POINT('Ctrl Pts',(0.106427098863261,-0.0622637901458048,
-1.21430643318376E-17));
#19625=CARTESIAN_POINT('Ctrl Pts',(0.104287070791936,-0.0651456752410043,
-1.32377232732828E-17));
#19626=CARTESIAN_POINT('Ctrl Pts',(0.102021590876101,-0.067943056099314,
-1.03088264066386E-17));
#19627=CARTESIAN_POINT('Ctrl Pts',(0.0996491962474235,-0.0706287444932102,
-1.04083408558608E-17));
#19628=CARTESIAN_POINT('Ctrl Pts',(0.0938611946766418,-0.0771810981592459,
-1.06511292104842E-17));
#19629=CARTESIAN_POINT('Ctrl Pts',(0.0874218747326319,-0.0830961188460978,
9.460259835177E-18));
#19630=CARTESIAN_POINT('Ctrl Pts',(0.0803902102994179,-0.0882260767030795,
2.94902990916057E-17));
#19631=CARTESIAN_POINT('Ctrl Pts',(0.0765868618375105,-0.091000813397402,
4.03243227742548E-17));
#19632=CARTESIAN_POINT('Ctrl Pts',(0.0726097989303321,-0.0935451549285004,
-2.49510848448888E-18));
#19633=CARTESIAN_POINT('Ctrl Pts',(0.0684664424539416,-0.0958295198918429,
0.));
#19634=CARTESIAN_POINT('Ctrl Pts',(-0.00156962371674571,0.146072546381438,
1.50365));
#19635=CARTESIAN_POINT('Ctrl Pts',(0.0218361081466035,0.146362061217761,
1.50238307892777));
#19636=CARTESIAN_POINT('Ctrl Pts',(0.0452966847593804,0.141345883428421,
1.50111615785553));
#19637=CARTESIAN_POINT('Ctrl Pts',(0.0660179268768178,0.130913916311315,
1.4998492367833));
#19638=CARTESIAN_POINT('Ctrl Pts',(0.109300214423576,0.109123745727819,
1.4972029069042));
#19639=CARTESIAN_POINT('Ctrl Pts',(0.140630685714559,0.0637042888941242,
1.49455657702509));
#19640=CARTESIAN_POINT('Ctrl Pts',(0.145752650840527,0.0155206226173656,
1.49191024714599));
#19641=CARTESIAN_POINT('Ctrl Pts',(0.150874615966495,-0.0326630436593903,
1.48926391726689));
#19642=CARTESIAN_POINT('Ctrl Pts',(0.129788074927449,-0.0836109193792113,
1.48661758738779));
#19643=CARTESIAN_POINT('Ctrl Pts',(0.0921021927661857,-0.114042242015571,
1.48397125750869));
#19644=CARTESIAN_POINT('Ctrl Pts',(0.0544163106049216,-0.144473564651931,
1.48132492762959));
#19645=CARTESIAN_POINT('Ctrl Pts',(0.000131087321441313,-0.154388334204831,
1.47867859775048));
#19646=CARTESIAN_POINT('Ctrl Pts',(-0.0458840977328367,-0.139228052523514,
1.47603226787138));
#19647=CARTESIAN_POINT('Ctrl Pts',(-0.0918992827871148,-0.124067770842196,
1.47338593799228));
#19648=CARTESIAN_POINT('Ctrl Pts',(-0.129644429612189,-0.0838324379266627,
1.47073960811318));
#19649=CARTESIAN_POINT('Ctrl Pts',(-0.141854649713415,-0.0369491035797489,
1.46809327823408));
#19650=CARTESIAN_POINT('Ctrl Pts',(-0.14497337938942,-0.0249741805295802,
1.46741735368415));
#19651=CARTESIAN_POINT('Ctrl Pts',(-0.146426231435716,-0.0125655473306973,
1.46674142913422));
#19652=CARTESIAN_POINT('Ctrl Pts',(-0.14631473222987,-0.000131398079681141,
1.46606550458429));
#19653=CARTESIAN_POINT('Origin',(0.,0.,-0.0924367114736175));
#19654=CARTESIAN_POINT('',(-0.0684664424539507,-0.0958295198918364,0.));
#19655=CARTESIAN_POINT('Ctrl Pts',(-0.0686146973663072,-0.0959584553529141,
8.16675286424706E-17));
#19656=CARTESIAN_POINT('Ctrl Pts',(-0.0391968190522335,-0.116741470120209,
0.00244290680874874));
#19657=CARTESIAN_POINT('Ctrl Pts',(0.0436301113039178,-0.130476273073809,
0.0075332029917574));
#19658=CARTESIAN_POINT('Ctrl Pts',(0.134092250525203,-0.0374520209666004,
0.0152708885490261));
#19659=CARTESIAN_POINT('Ctrl Pts',(0.104134301645602,0.0924305194826295,
0.023213056671806));
#19660=CARTESIAN_POINT('Ctrl Pts',(-0.0212379681243542,0.137589894578696,
0.0311552247945861));
#19661=CARTESIAN_POINT('Ctrl Pts',(-0.106685947947232,0.0723488109778776,
0.0375631097285225));
#19662=CARTESIAN_POINT('Ctrl Pts',(-0.117663533972591,0.0165813593984342,
0.041323605288199));
#19663=CARTESIAN_POINT('Ctrl Pts',(-0.117600989619072,5.04992496179954E-5,
0.0424367114736154));
#19664=CARTESIAN_POINT('Origin',(0.,0.,0.));
#19665=CARTESIAN_POINT('Ctrl Pts',(-0.0510216505388318,0.106149619882943,
-0.0164977839420939));
#19666=CARTESIAN_POINT('Ctrl Pts',(-0.0863355867949722,0.0891756983861136,
-0.0138503945678339));
#19667=CARTESIAN_POINT('Ctrl Pts',(-0.13808023131828,0.0175094743621551,
-0.00855561581931395));
#19668=CARTESIAN_POINT('Ctrl Pts',(-0.0894531427980795,-0.106808298616542,
-0.000613447696533924));
#19669=CARTESIAN_POINT('Ctrl Pts',(0.0412394829729132,-0.132934609947913,
0.00732872042624606));
#19670=CARTESIAN_POINT('Ctrl Pts',(0.134092250525203,-0.0374520209666004,
0.0152708885490261));
#19671=CARTESIAN_POINT('Ctrl Pts',(0.104134301645602,0.0924305194826295,
0.023213056671806));
#19672=CARTESIAN_POINT('Ctrl Pts',(-0.0212379681243542,0.137589894578696,
0.0311552247945861));
#19673=CARTESIAN_POINT('Ctrl Pts',(-0.127145335141994,0.0567276974868182,
0.039097392917366));
#19674=CARTESIAN_POINT('Ctrl Pts',(-0.116579117211717,-0.0761160149501382,
0.0470395610401461));
#19675=CARTESIAN_POINT('Ctrl Pts',(0.000787973702835166,-0.139222729671589,
0.054981729162926));
#19676=CARTESIAN_POINT('Ctrl Pts',(0.117431922513572,-0.0747907597173192,
0.0629238972857061));
#19677=CARTESIAN_POINT('Ctrl Pts',(0.126496838785129,0.0581591461343325,
0.070866065408486));
#19678=CARTESIAN_POINT('Ctrl Pts',(0.0196773008918215,0.137828289815661,
0.0788082335312661));
#19679=CARTESIAN_POINT('Ctrl Pts',(-0.105168479521776,0.0912330920368172,
0.0867504016540459));
#19680=CARTESIAN_POINT('Ctrl Pts',(-0.133669226619255,-0.0389412707994331,
0.0946925697768262));
#19681=CARTESIAN_POINT('Ctrl Pts',(-0.0397151780004399,-0.133441281507892,
0.102634737899606));
#19682=CARTESIAN_POINT('Ctrl Pts',(0.0906220264938673,-0.105695447092796,
0.110576906022386));
#19683=CARTESIAN_POINT('Ctrl Pts',(0.137940159127448,0.0188783162799928,
0.118519074145166));
#19684=CARTESIAN_POINT('Ctrl Pts',(0.0588909273047484,0.126157580947307,
0.126461242267946));
#19685=CARTESIAN_POINT('Ctrl Pts',(-0.074108440039672,0.117863552156501,
0.134403410390726));
#19686=CARTESIAN_POINT('Ctrl Pts',(-0.139216864956951,0.00159439502933392,
0.142345578513506));
#19687=CARTESIAN_POINT('Ctrl Pts',(-0.0767883381764272,-0.116135388594389,
0.150287746636286));
#19688=CARTESIAN_POINT('Ctrl Pts',(0.0559861945572589,-0.127473226882309,
0.158229914759066));
#19689=CARTESIAN_POINT('Ctrl Pts',(0.137471621702818,-0.0220324926503626,
0.166172082881846));
#19690=CARTESIAN_POINT('Ctrl Pts',(0.0930189202108026,0.103592267873211,
0.174114251004626));
#19691=CARTESIAN_POINT('Ctrl Pts',(-0.0366486683060043,0.134315868829211,
0.182056419127406));
#19692=CARTESIAN_POINT('Ctrl Pts',(-0.132742311638566,0.0419923350165386,
0.189998587250186));
#19693=CARTESIAN_POINT('Ctrl Pts',(-0.107230360350792,-0.0888004916405464,
0.197940755372966));
#19694=CARTESIAN_POINT('Ctrl Pts',(0.0165156171993534,-0.138242945169174,
0.205882923495746));
#19695=CARTESIAN_POINT('Ctrl Pts',(0.125131592687617,-0.061040658666823,
0.213825091618526));
#19696=CARTESIAN_POINT('Ctrl Pts',(0.119114174013628,0.0720811421096423,
0.221767259741306));
#19697=CARTESIAN_POINT('Ctrl Pts',(0.0039759348809324,0.139169211541763,
0.229709427864086));
#19698=CARTESIAN_POINT('Ctrl Pts',(-0.114804669066963,0.0787639858025777,
0.237651595986866));
#19699=CARTESIAN_POINT('Ctrl Pts',(-0.128412401817242,-0.0537971426620367,
0.245593764109646));
#19700=CARTESIAN_POINT('Ctrl Pts',(-0.024381182195918,-0.137074561658528,
0.253535932232426));
#19701=CARTESIAN_POINT('Ctrl Pts',(0.101985705091022,-0.094777599970642,
0.261478100355206));
#19702=CARTESIAN_POINT('Ctrl Pts',(0.134923209124943,0.0343453801629359,
0.269420268477986));
#19703=CARTESIAN_POINT('Ctrl Pts',(0.0442571924125319,0.132004463632409,
0.277362436600766));
#19704=CARTESIAN_POINT('Ctrl Pts',(-0.0869529592639067,0.108733897080731,
0.285304604723546));
#19705=CARTESIAN_POINT('Ctrl Pts',(-0.138505267237684,-0.0141480898545381,
0.293246772846326));
#19706=CARTESIAN_POINT('Ctrl Pts',(-0.0631725212350128,-0.124068972994571,
0.301188940969106));
#19707=CARTESIAN_POINT('Ctrl Pts',(0.0700327441786229,-0.12032993078169,
0.309131109091886));
#19708=CARTESIAN_POINT('Ctrl Pts',(0.139080821187468,-0.00635631000930847,
0.317073277214666));
#19709=CARTESIAN_POINT('Ctrl Pts',(0.0807165776729536,0.11344034374014,
0.325015445337446));
#19710=CARTESIAN_POINT('Ctrl Pts',(-0.0515923433190751,0.129313988454311,
0.332957613460226));
#19711=CARTESIAN_POINT('Ctrl Pts',(-0.136637377548019,0.026722734813544,
0.340899781583006));
#19712=CARTESIAN_POINT('Ctrl Pts',(-0.0965085366518414,-0.100349289247285,
0.348841949705786));
#19713=CARTESIAN_POINT('Ctrl Pts',(0.0320320385160992,-0.135491055083419,
0.356784117828566));
#19714=CARTESIAN_POINT('Ctrl Pts',(0.131227975626944,-0.0465090949381858,
0.364726285951346));
#19715=CARTESIAN_POINT('Ctrl Pts',(0.110205605501345,0.0850799742312894,
0.372668454074126));
#19716=CARTESIAN_POINT('Ctrl Pts',(-0.0117764211155082,0.138727046407055,
0.380610622196906));
#19717=CARTESIAN_POINT('Ctrl Pts',(-0.122970036152848,0.065285892102983,
0.388552790319686));
#19718=CARTESIAN_POINT('Ctrl Pts',(-0.121510464882371,-0.0679638464419502,
0.396494958442466));
#19719=CARTESIAN_POINT('Ctrl Pts',(-0.00873482453528946,-0.138951719454826,
0.404437126565246));
#19720=CARTESIAN_POINT('Ctrl Pts',(0.112042812448737,-0.0826455423945668,
0.412379294688026));
#19721=CARTESIAN_POINT('Ctrl Pts',(0.130177722634257,0.049372441998279,
0.420321462810806));
#19722=CARTESIAN_POINT('Ctrl Pts',(0.0290564652212241,0.136160197297018,
0.428263630933586));
#19723=CARTESIAN_POINT('Ctrl Pts',(-0.098683499418539,0.098211223603141,
0.436205799056366));
#19724=CARTESIAN_POINT('Ctrl Pts',(-0.136019240449831,-0.0297093205335648,
0.444147967179146));
#19725=CARTESIAN_POINT('Ctrl Pts',(-0.0487473834415776,-0.130413074907061,
0.452090135301926));
#19726=CARTESIAN_POINT('Ctrl Pts',(0.0831820848081396,-0.111645054821459,
0.460032303424706));
#19727=CARTESIAN_POINT('Ctrl Pts',(0.138908217753341,0.00940130521287039,
0.467974471547486));
#19728=CARTESIAN_POINT('Ctrl Pts',(0.0673801526530663,0.121835103839429,
0.475916639670265));
#19729=CARTESIAN_POINT('Ctrl Pts',(-0.0658750545035054,0.12265543075329,
0.483858807793047));
#19730=CARTESIAN_POINT('Ctrl Pts',(-0.138781944133385,0.0111107822259715,
0.491800975915825));
#19731=CARTESIAN_POINT('Ctrl Pts',(-0.084550315326251,-0.110612484274364,
0.499743144038607));
#19732=CARTESIAN_POINT('Ctrl Pts',(0.0471380885036503,-0.131003351527116,
0.507685312161385));
#19733=CARTESIAN_POINT('Ctrl Pts',(0.135643160584381,-0.031381690295376,
0.515627480284167));
#19734=CARTESIAN_POINT('Ctrl Pts',(0.0998851624184703,0.0969888232104648,
0.523569648406945));
#19735=CARTESIAN_POINT('Ctrl Pts',(-0.0273779061153799,0.136507610615132,
0.531511816529727));
#19736=CARTESIAN_POINT('Ctrl Pts',(-0.129560000008381,0.0509714027366644,
0.539453984652505));
#19737=CARTESIAN_POINT('Ctrl Pts',(-0.113051823689188,-0.0812598465397498,
0.547396152775286));
#19738=CARTESIAN_POINT('Ctrl Pts',(0.00702343738442799,-0.139048728244533,
0.555338320898066));
#19739=CARTESIAN_POINT('Ctrl Pts',(0.12066450826877,-0.0694546898587181,
0.563280489020846));
#19740=CARTESIAN_POINT('Ctrl Pts',(0.123764493242992,0.063766979789076,
0.571222657143626));
#19741=CARTESIAN_POINT('Ctrl Pts',(0.0134834875971477,0.13857154491934,
0.579164825266405));
#19742=CARTESIAN_POINT('Ctrl Pts',(-0.109149777898995,0.0864303389077871,
0.587106993389186));
#19743=CARTESIAN_POINT('Ctrl Pts',(-0.131790633456927,-0.0448899368693808,
0.595049161511966));
#19744=CARTESIAN_POINT('Ctrl Pts',(-0.0336977294021144,-0.135086418755761,
0.602991329634746));
#19745=CARTESIAN_POINT('Ctrl Pts',(0.0952657566843092,-0.101529863106778,
0.610933497757526));
#19746=CARTESIAN_POINT('Ctrl Pts',(0.136956022624868,0.025038477707157,
0.618875665880307));
#19747=CARTESIAN_POINT('Ctrl Pts',(0.0531805018142573,0.128669000640787,
0.626817834003085));
#19748=CARTESIAN_POINT('Ctrl Pts',(-0.0793138220987445,0.114425500318782,
0.634760002125867));
#19749=CARTESIAN_POINT('Ctrl Pts',(-0.139148536750765,-0.00464351367351466,
0.642702170248646));
#19750=CARTESIAN_POINT('Ctrl Pts',(-0.0715088964667609,-0.119458592094588,
0.650644338371427));
#19751=CARTESIAN_POINT('Ctrl Pts',(0.0616402393688536,-0.124837327709565,
0.658586506494205));
#19752=CARTESIAN_POINT('Ctrl Pts',(0.138320583400205,-0.0158522461166236,
0.666528674616987));
#19753=CARTESIAN_POINT('Ctrl Pts',(0.0882850628235238,0.107655121482266,
0.674470842739765));
#19754=CARTESIAN_POINT('Ctrl Pts',(-0.0426286451686149,0.132539337972556,
0.682413010862546));
#19755=CARTESIAN_POINT('Ctrl Pts',(-0.13449013477919,0.0360039045964495,
0.690355178985326));
#19756=CARTESIAN_POINT('Ctrl Pts',(-0.103144844235522,-0.0935148042116587,
0.698297347108106));
#19757=CARTESIAN_POINT('Ctrl Pts',(0.022691720100341,-0.137364345221032,
0.706239515230886));
#19758=CARTESIAN_POINT('Ctrl Pts',(0.127740337615313,-0.0553740340325759,
0.714181683353665));
#19759=CARTESIAN_POINT('Ctrl Pts',(0.115765682611161,0.077344581120379,
0.722123851476446));
#19760=CARTESIAN_POINT('Ctrl Pts',(-0.00226223072526165,0.139207614056346,
0.730066019599226));
#19761=CARTESIAN_POINT('Ctrl Pts',(-0.118217708309552,0.0735421711751344,
0.738008187722006));
#19762=CARTESIAN_POINT('Ctrl Pts',(-0.125873620115675,-0.059495455776806,
0.745950355844786));
#19763=CARTESIAN_POINT('Ctrl Pts',(-0.0182163644075178,-0.138029133036789,
0.753892523967566));
#19764=CARTESIAN_POINT('Ctrl Pts',(0.106128952536144,-0.0901139441634624,
0.761834692090347));
#19765=CARTESIAN_POINT('Ctrl Pts',(0.133249245915149,0.0403548753208232,
0.769776860213125));
#19766=CARTESIAN_POINT('Ctrl Pts',(0.0382995408207276,0.133854483197375,
0.777719028335907));
#19767=CARTESIAN_POINT('Ctrl Pts',(-0.0917364783268051,0.104729633071593,
0.785661196458685));
#19768=CARTESIAN_POINT('Ctrl Pts',(-0.137732458880487,-0.0203383202317681,
0.793603364581467));
#19769=CARTESIAN_POINT('Ctrl Pts',(-0.0575513573065257,-0.126774282767806,
0.801545532704245));
#19770=CARTESIAN_POINT('Ctrl Pts',(0.0753527000357912,-0.117071978271622,
0.809487700827026));
#19771=CARTESIAN_POINT('Ctrl Pts',(0.139225942868322,-0.000119714417332432,
0.817429868949805));
#19772=CARTESIAN_POINT('Ctrl Pts',(0.0755539188089132,0.116942220141962,
0.825372037072586));
#19773=CARTESIAN_POINT('Ctrl Pts',(-0.0573332568284509,0.12687306712048,
0.833314205195366));
#19774=CARTESIAN_POINT('Ctrl Pts',(-0.13769727914169,0.0205751504512258,
0.841256373318145));
#19775=CARTESIAN_POINT('Ctrl Pts',(-0.0919164475821765,-0.104571717796869,
0.849198541440926));
#19776=CARTESIAN_POINT('Ctrl Pts',(0.0380692928980519,-0.133920149482284,
0.857140709563706));
#19777=CARTESIAN_POINT('Ctrl Pts',(0.133179650076608,-0.0405839661022353,
0.865082877686486));
#19778=CARTESIAN_POINT('Ctrl Pts',(0.106283765719693,0.0899312995767124,
0.873025045809266));
#19779=CARTESIAN_POINT('Ctrl Pts',(-0.0179789669825735,0.138060255849953,
0.880967213932046));
#19780=CARTESIAN_POINT('Ctrl Pts',(-0.125771118879347,0.0597118342956578,
0.888909382054826));
#19781=CARTESIAN_POINT('Ctrl Pts',(-0.118344004924669,-0.0733387619032726,
0.896851550177606));
#19782=CARTESIAN_POINT('Ctrl Pts',(-0.00250162451743248,-0.139203517821528,
0.904793718300386));
#19783=CARTESIAN_POINT('Ctrl Pts',(0.115632500949424,-0.0775435504945224,
0.912735886423165));
#19784=CARTESIAN_POINT('Ctrl Pts',(0.127835376168433,0.0551542754370876,
0.920678054545947));
#19785=CARTESIAN_POINT('Ctrl Pts',(0.0229279137899797,0.137325118854324,
0.928620222668725));
#19786=CARTESIAN_POINT('Ctrl Pts',(-0.102983873094174,0.0936920454555137,
0.936562390791507));
#19787=CARTESIAN_POINT('Ctrl Pts',(-0.134551852288801,-0.0357725669300891,
0.944504558914285));
#19788=CARTESIAN_POINT('Ctrl Pts',(-0.0428565117498991,-0.132465832952297,
0.952446727037066));
#19789=CARTESIAN_POINT('Ctrl Pts',(0.0880997963686447,-0.107806787258123,
0.960388895159846));
#19790=CARTESIAN_POINT('Ctrl Pts',(0.138347640177547,0.0156143509765511,
0.968331063282625));
#19791=CARTESIAN_POINT('Ctrl Pts',(0.061854832590724,0.124731139593481,
0.976273231405407));
#19792=CARTESIAN_POINT('Ctrl Pts',(-0.0713033562375951,0.119581390225944,
0.984215399528185));
#19793=CARTESIAN_POINT('Ctrl Pts',(-0.139140345480169,0.00488280234845834,
0.992157567650966));
#19794=CARTESIAN_POINT('Ctrl Pts',(-0.0795104838321055,-0.114288934109561,
1.00009973577375));
#19795=CARTESIAN_POINT('Ctrl Pts',(0.0529591494285269,-0.128760265574912,
1.00804190389653));
#19796=CARTESIAN_POINT('Ctrl Pts',(0.136912761112491,-0.0252739657289669,
1.0159840720193));
#19797=CARTESIAN_POINT('Ctrl Pts',(0.0954402180350474,0.101365883217864,
1.02392624014209));
#19798=CARTESIAN_POINT('Ctrl Pts',(-0.0334653697086341,0.135144169424284,
1.03186840826486));
#19799=CARTESIAN_POINT('Ctrl Pts',(-0.131713240771149,0.0451165125500212,
1.03981057638765));
#19800=CARTESIAN_POINT('Ctrl Pts',(-0.109298251871946,-0.0862425048155002,
1.04775274451043));
#19801=CARTESIAN_POINT('Ctrl Pts',(0.0132451643780021,-0.13859452774087,
1.05569491263321));
#19802=CARTESIAN_POINT('Ctrl Pts',(0.123654649330263,-0.0639797248987874,
1.06363708075599));
#19803=CARTESIAN_POINT('Ctrl Pts',(0.120783771971213,0.0692470788374567,
1.07157924887876));
#19804=CARTESIAN_POINT('Ctrl Pts',(0.00726255089817806,0.139036444335888,
1.07952141700155));
#19805=CARTESIAN_POINT('Ctrl Pts',(-0.112911912907791,0.0814541430660127,
1.08746358512433));
#19806=CARTESIAN_POINT('Ctrl Pts',(-0.129647464608677,-0.0507485213543897,
1.09540575324711));
#19807=CARTESIAN_POINT('Ctrl Pts',(-0.0276126195379174,-0.136460326620484,
1.10334792136989));
#19808=CARTESIAN_POINT('Ctrl Pts',(0.0997182217817603,-0.0971604536002107,
1.11129008949267));
#19809=CARTESIAN_POINT('Ctrl Pts',(0.135696927507188,0.0311483765905046,
1.11923225761545));
#19810=CARTESIAN_POINT('Ctrl Pts',(0.0473633069609982,0.130922093830007,
1.12717442573822));
#19811=CARTESIAN_POINT('Ctrl Pts',(-0.0843599685788644,0.110757722983492,
1.13511659386101));
#19812=CARTESIAN_POINT('Ctrl Pts',(-0.138800846271631,-0.0108721006891078,
1.14305876198379));
#19813=CARTESIAN_POINT('Ctrl Pts',(-0.0660858892268601,-0.122541963197144,
1.15100093010657));
#19814=CARTESIAN_POINT('Ctrl Pts',(0.0671705316110708,-0.121950798202395,
1.15894309822935));
#19815=CARTESIAN_POINT('Ctrl Pts',(0.138891844802359,-0.00964017357273747,
1.16688526635212));
#19816=CARTESIAN_POINT('Ctrl Pts',(0.0833739592533277,0.111501840422208,
1.17482743447491));
#19817=CARTESIAN_POINT('Ctrl Pts',(-0.0485230383040216,0.130496713571114,
1.18276960259768));
#19818=CARTESIAN_POINT('Ctrl Pts',(-0.135967947813762,0.0299431906521225,
1.19071177072047));
#19819=CARTESIAN_POINT('Ctrl Pts',(-0.0988522486080867,-0.0980413710850678,
1.19865393884324));
#19820=CARTESIAN_POINT('Ctrl Pts',(0.0288222657999454,-0.136209964735594,
1.20659610696603));
#19821=CARTESIAN_POINT('Ctrl Pts',(0.130092623711363,-0.0495962373069701,
1.21453827508881));
#19822=CARTESIAN_POINT('Ctrl Pts',(0.112184773380136,0.082452738709893,
1.22248044321158));
#19823=CARTESIAN_POINT('Ctrl Pts',(-0.00849585454694533,0.138966535376798,
1.23042261133437));
#19824=CARTESIAN_POINT('Ctrl Pts',(-0.121393406896754,0.0681727090639588,
1.23836477945715));
#19825=CARTESIAN_POINT('Ctrl Pts',(-0.123082127310551,-0.0650743223999996,
1.24630694757992));
#19826=CARTESIAN_POINT('Ctrl Pts',(-0.0120149744006178,-0.138706589206355,
1.25424911570271));
#19827=CARTESIAN_POINT('Ctrl Pts',(0.110059129405696,-0.0852693704304675,
1.26219128382548));
#19828=CARTESIAN_POINT('Ctrl Pts',(0.13130776387206,0.0462833517151888,
1.27013345194827));
#19829=CARTESIAN_POINT('Ctrl Pts',(0.0322649968732001,0.135435768819968,
1.27807562007105));
#19830=CARTESIAN_POINT('Ctrl Pts',(-0.0963358219719167,0.100515107841202,
1.28601778819382));
#19831=CARTESIAN_POINT('Ctrl Pts',(-0.136683130933199,-0.0264877182308561,
1.29395995631661));
#19832=CARTESIAN_POINT('Ctrl Pts',(-0.0518146499729274,-0.129225073214149,
1.30190212443939));
#19833=CARTESIAN_POINT('Ctrl Pts',(0.0805213734929343,-0.11357898534207,
1.30984429256217));
#19834=CARTESIAN_POINT('Ctrl Pts',(0.1390915465469,0.0061171215252809,1.31778646068495));
#19835=CARTESIAN_POINT('Ctrl Pts',(0.0702395735793815,0.120209316621791,
1.32572862880773));
#19836=CARTESIAN_POINT('Ctrl Pts',(-0.0629590648350173,0.124177428154433,
1.33367079693051));
#19837=CARTESIAN_POINT('Ctrl Pts',(-0.138480731711197,0.0143862582011507,
1.34161296505328));
#19838=CARTESIAN_POINT('Ctrl Pts',(-0.0871398218994898,-0.108584202098263,
1.34955513317607));
#19839=CARTESIAN_POINT('Ctrl Pts',(0.0440301174146577,-0.132080378229483,
1.35749730129884));
#19840=CARTESIAN_POINT('Ctrl Pts',(0.13486394497766,-0.0345773583278084,
1.36543946942163));
#19841=CARTESIAN_POINT('Ctrl Pts',(0.102148545386143,0.0946020732301706,
1.3733816375444));
#19842=CARTESIAN_POINT('Ctrl Pts',(-0.0241454188302812,0.137116288461919,
1.38132380566719));
#19843=CARTESIAN_POINT('Ctrl Pts',(-0.128319693277533,0.0540178939468163,
1.38926597378996));
#19844=CARTESIAN_POINT('Ctrl Pts',(-0.114939956470138,-0.0785664351508689,
1.39720814191275));
#19845=CARTESIAN_POINT('Ctrl Pts',(0.00373660876362508,-0.139175849115243,
1.40515031003553));
#19846=CARTESIAN_POINT('Ctrl Pts',(0.118990018389619,-0.0722858665142316,
1.41309247815831));
#19847=CARTESIAN_POINT('Ctrl Pts',(0.125236419206141,0.0608253567263532,
1.42103464628109));
#19848=CARTESIAN_POINT('Ctrl Pts',(0.0167532566496359,0.13821437898841,
1.42897681440387));
#19849=CARTESIAN_POINT('Ctrl Pts',(-0.107077349343502,0.0889846891406984,
1.43691898252665));
#19850=CARTESIAN_POINT('Ctrl Pts',(-0.132814597987359,-0.0417638487589672,
1.44486115064943));
#19851=CARTESIAN_POINT('Ctrl Pts',(-0.0368790902657646,-0.134252921254984,
1.45280331877221));
#19852=CARTESIAN_POINT('Ctrl Pts',(0.0928396680879532,-0.103751556080299,
1.46074548689499));
#19853=CARTESIAN_POINT('Ctrl Pts',(0.137511141307062,0.0217950526079239,
1.46868765501776));
#19854=CARTESIAN_POINT('Ctrl Pts',(0.0562018483347667,0.127378648737854,
1.47662982314055));
#19855=CARTESIAN_POINT('Ctrl Pts',(-0.0765818961642769,0.116263681173923,
1.48457199126332));
#19856=CARTESIAN_POINT('Ctrl Pts',(-0.13923195096087,-0.00134816270381636,
1.49251415938611));
#19857=CARTESIAN_POINT('Ctrl Pts',(-0.0742871760264013,-0.117748889605885,
1.50045632750888));
#19858=CARTESIAN_POINT('Ctrl Pts',(0.0586284551779338,-0.126233948370975,
1.50839849563167));
#19859=CARTESIAN_POINT('Ctrl Pts',(0.137995068118234,-0.019163470063063,
1.51634066375444));
#19860=CARTESIAN_POINT('Ctrl Pts',(0.0906261803825392,0.105639137646141,
1.52428283187723));
#19861=CARTESIAN_POINT('Ctrl Pts',(0.00417072711528833,0.124051375507138,
1.52957761062575));
#19862=CARTESIAN_POINT('Ctrl Pts',(-0.0334019664627544,0.1129391839063,
1.53222500000001));
#19863=CARTESIAN_POINT('Ctrl Pts',(-0.0551480035117261,0.114734422509858,
-0.0109985226280628));
#19864=CARTESIAN_POINT('Ctrl Pts',(-0.093317938433455,0.0963877427684319,
-0.00835113325380276));
#19865=CARTESIAN_POINT('Ctrl Pts',(-0.149247407742026,0.0189255452031589,
-0.00305635450528277));
#19866=CARTESIAN_POINT('Ctrl Pts',(-0.0966876253720675,-0.115446371588928,
0.00488581361749726));
#19867=CARTESIAN_POINT('Ctrl Pts',(0.0445747075563756,-0.143685636564375,
0.0128279817402772));
#19868=CARTESIAN_POINT('Ctrl Pts',(0.144936900801175,-0.0404809362687151,
0.0207701498630572));
#19869=CARTESIAN_POINT('Ctrl Pts',(0.112556116319125,0.0999057960529736,
0.0287123179858373));
#19870=CARTESIAN_POINT('Ctrl Pts',(-0.0229555792165621,0.148717415239805,
0.0366544861086172));
#19871=CARTESIAN_POINT('Ctrl Pts',(-0.137428156769908,0.0613155244327884,
0.0445966542313972));
#19872=CARTESIAN_POINT('Ctrl Pts',(-0.126007400730642,-0.0822718633254329,
0.0525388223541772));
#19873=CARTESIAN_POINT('Ctrl Pts',(0.000851700720621877,-0.150482305134309,
0.0604809904769572));
#19874=CARTESIAN_POINT('Ctrl Pts',(0.126929176276611,-0.0808394286734405,
0.0684231585997372));
#19875=CARTESIAN_POINT('Ctrl Pts',(0.136727213562698,0.0628627408439891,
0.0763653267225173));
#19876=CARTESIAN_POINT('Ctrl Pts',(0.0212686937255662,0.148975090584026,
0.0843074948452972));
#19877=CARTESIAN_POINT('Ctrl Pts',(-0.113673932864549,0.0986115272026031,
0.0922496629680772));
#19878=CARTESIAN_POINT('Ctrl Pts',(-0.144479665027646,-0.0420906285100245,
0.100191831090857));
#19879=CARTESIAN_POINT('Ctrl Pts',(-0.0429271251068198,-0.144233284958223,
0.108133999213637));
#19880=CARTESIAN_POINT('Ctrl Pts',(0.0979510420095061,-0.114243518700172,
0.116076167336417));
#19881=CARTESIAN_POINT('Ctrl Pts',(0.149096007275942,0.0204050915936607,
0.124018335459197));
#19882=CARTESIAN_POINT('Ctrl Pts',(0.0636537044864716,0.136360518400275,
0.131960503581977));
#19883=CARTESIAN_POINT('Ctrl Pts',(-0.0801019266996435,0.127395713772213,
0.139902671704757));
#19884=CARTESIAN_POINT('Ctrl Pts',(-0.15047596611352,0.00172334100814176,
0.147844839827537));
#19885=CARTESIAN_POINT('Ctrl Pts',(-0.0829985603893774,-0.125527785761544,
0.155787007950317));
#19886=CARTESIAN_POINT('Ctrl Pts',(0.0605140527882773,-0.137782566606816,
0.163729176073097));
#19887=CARTESIAN_POINT('Ctrl Pts',(0.148589577098441,-0.0238143605552183,
0.171671344195877));
#19888=CARTESIAN_POINT('Ctrl Pts',(0.100541783424623,0.111970245809892,
0.179613512318657));
#19889=CARTESIAN_POINT('Ctrl Pts',(-0.0396126128240685,0.145178604134651,
0.187555680441437));
#19890=CARTESIAN_POINT('Ctrl Pts',(-0.143477786216001,0.0453884461694337,
0.195497848564217));
#19891=CARTESIAN_POINT('Ctrl Pts',(-0.115902567375552,-0.095982191346566,
0.203440016686997));
#19892=CARTESIAN_POINT('Ctrl Pts',(0.0178513102906219,-0.149423281002214,
0.211382184809777));
#19893=CARTESIAN_POINT('Ctrl Pts',(0.135251553802876,-0.0659772944027704,
0.219324352932557));
#19894=CARTESIAN_POINT('Ctrl Pts',(0.128747479107914,0.07791067196398,0.227266521055337));
#19895=CARTESIAN_POINT('Ctrl Pts',(0.00429748682099232,0.150424458749874,
0.235208689178117));
#19896=CARTESIAN_POINT('Ctrl Pts',(-0.124089444892588,0.0851339876261335,
0.243150857300897));
#19897=CARTESIAN_POINT('Ctrl Pts',(-0.138797696890977,-0.0581479623084488,
0.251093025423677));
#19898=CARTESIAN_POINT('Ctrl Pts',(-0.0263529993083425,-0.148160405002171,
0.259035193546457));
#19899=CARTESIAN_POINT('Ctrl Pts',(0.110233752987369,-0.102442695616748,
0.266977361669237));
#19900=CARTESIAN_POINT('Ctrl Pts',(0.145835062802846,0.0371230472913779,
0.274919529792017));
#19901=CARTESIAN_POINT('Ctrl Pts',(0.0478364728857143,0.142680265085169,
0.282861697914797));
#19902=CARTESIAN_POINT('Ctrl Pts',(-0.0939852406223356,0.117527701960322,
0.290803866037577));
#19903=CARTESIAN_POINT('Ctrl Pts',(-0.14970681824969,-0.01529231023972,
0.298746034160357));
#19904=CARTESIAN_POINT('Ctrl Pts',(-0.0682815703945392,-0.134102995221473,
0.306688202283137));
#19905=CARTESIAN_POINT('Ctrl Pts',(0.0756966107742644,-0.1300615596562,
0.314630370405917));
#19906=CARTESIAN_POINT('Ctrl Pts',(0.150328919865546,-0.00687037371415525,
0.322572538528697));
#19907=CARTESIAN_POINT('Ctrl Pts',(0.0872444944832666,0.122614780370367,
0.330514706651477));
#19908=CARTESIAN_POINT('Ctrl Pts',(-0.0557648508131485,0.139772198940638,
0.338456874774257));
#19909=CARTESIAN_POINT('Ctrl Pts',(-0.147687863823926,0.0288839239377102,
0.346399042897038));
#19910=CARTESIAN_POINT('Ctrl Pts',(-0.104313621021262,-0.10846499275041,
0.354341211019817));
#19911=CARTESIAN_POINT('Ctrl Pts',(0.0346226151823369,-0.146448833047075,
0.362283379142597));
#19912=CARTESIAN_POINT('Ctrl Pts',(0.141840978962514,-0.0502704970123603,
0.370225547265377));
#19913=CARTESIAN_POINT('Ctrl Pts',(0.119118434135606,0.0919607787700563,
0.378167715388157));
#19914=CARTESIAN_POINT('Ctrl Pts',(-0.0127288338612142,0.149946533709345,
0.386109883510937));
#19915=CARTESIAN_POINT('Ctrl Pts',(-0.132915182358376,0.070565859178174,
0.394052051633717));
#19916=CARTESIAN_POINT('Ctrl Pts',(-0.131337568919768,-0.0734603918663599,
0.401994219756497));
#19917=CARTESIAN_POINT('Ctrl Pts',(-0.00944124952954395,-0.150189377088511,
0.409936387879277));
#19918=CARTESIAN_POINT('Ctrl Pts',(0.121104224366159,-0.0893294633566384,
0.417878556002057));
#19919=CARTESIAN_POINT('Ctrl Pts',(0.140705787232781,0.0533654159743681,
0.425820724124838));
#19920=CARTESIAN_POINT('Ctrl Pts',(0.0314063937394313,0.147172091835368,
0.433762892247617));
#19921=CARTESIAN_POINT('Ctrl Pts',(-0.106664482920656,0.106154012011714,
0.441705060370398));
#19922=CARTESIAN_POINT('Ctrl Pts',(-0.147019735166745,-0.032112048430678,
0.449647228493177));
#19923=CARTESIAN_POINT('Ctrl Pts',(-0.052689806088835,-0.14096017351449,
0.457589396615958));
#19924=CARTESIAN_POINT('Ctrl Pts',(0.0899093983958942,-0.120674298270189,
0.465531564738737));
#19925=CARTESIAN_POINT('Ctrl Pts',(0.15014235720654,0.0101616315312987,
0.473473732861518));
#19926=CARTESIAN_POINT('Ctrl Pts',(0.0728294921055832,0.131688462906045,
0.481415900984297));
#19927=CARTESIAN_POINT('Ctrl Pts',(-0.071202669822089,0.132575133389036,
0.489358069107078));
#19928=CARTESIAN_POINT('Ctrl Pts',(-0.150005871264529,0.012009361726732,
0.497300237229857));
#19929=CARTESIAN_POINT('Ctrl Pts',(-0.0913882839399832,-0.119558219045865,
0.505242405352637));
#19930=CARTESIAN_POINT('Ctrl Pts',(0.0509503601487159,-0.141598188489932,
0.513184573475417));
#19931=CARTESIAN_POINT('Ctrl Pts',(0.146613240011817,-0.0339196703426114,
0.521126741598197));
#19932=CARTESIAN_POINT('Ctrl Pts',(0.107963329873666,0.104832750538675,
0.529068909720978));
#19933=CARTESIAN_POINT('Ctrl Pts',(-0.0295920819230583,0.147547602048875,
0.537011077843756));
#19934=CARTESIAN_POINT('Ctrl Pts',(-0.140038106568177,0.055093691941219,
0.544953245966537));
#19935=CARTESIAN_POINT('Ctrl Pts',(-0.122194838935542,-0.0878316999746162,
0.552895414089317));
#19936=CARTESIAN_POINT('Ctrl Pts',(0.00759145471482065,-0.150294231420327,
0.560837582212097));
#19937=CARTESIAN_POINT('Ctrl Pts',(0.130423195946632,-0.0750718065719766,
0.568779750334878));
#19938=CARTESIAN_POINT('Ctrl Pts',(0.133773890807325,0.0689241055160235,
0.576721918457657));
#19939=CARTESIAN_POINT('Ctrl Pts',(0.0145739585745413,0.149778456108953,
0.584664086580438));
#19940=CARTESIAN_POINT('Ctrl Pts',(-0.117977216952174,0.0934203535806499,
0.592606254703216));
#19941=CARTESIAN_POINT('Ctrl Pts',(-0.142449141490696,-0.0485203902651028,
0.600548422825998));
#19942=CARTESIAN_POINT('Ctrl Pts',(-0.036423018067407,-0.146011471938939,
0.608490590948776));
#19943=CARTESIAN_POINT('Ctrl Pts',(0.102970331784443,-0.109741044988262,
0.616432759071558));
#19944=CARTESIAN_POINT('Ctrl Pts',(0.148032279177632,0.0270634532975707,
0.624374927194337));
#19945=CARTESIAN_POINT('Ctrl Pts',(0.0574814509102497,0.139075048028633,
0.632317095317117));
#19946=CARTESIAN_POINT('Ctrl Pts',(-0.0857282916847416,0.123679611042927,
0.640259263439898));
#19947=CARTESIAN_POINT('Ctrl Pts',(-0.150402111894479,-0.00501905574730406,
0.648201431562677));
#19948=CARTESIAN_POINT('Ctrl Pts',(-0.0772921462128499,-0.129119751845818,
0.656143599685457));
#19949=CARTESIAN_POINT('Ctrl Pts',(0.0666253659236285,-0.134933490277457,
0.664085767808237));
#19950=CARTESIAN_POINT('Ctrl Pts',(0.14950719819016,-0.0171342893707992,
0.672027935931017));
#19951=CARTESIAN_POINT('Ctrl Pts',(0.0954250774564579,0.11636168087194,
0.679970104053797));
#19952=CARTESIAN_POINT('Ctrl Pts',(-0.0460762176180427,0.143258397146306,
0.687912272176577));
#19953=CARTESIAN_POINT('Ctrl Pts',(-0.145366963764729,0.0389157041403328,
0.695854440299358));
#19954=CARTESIAN_POINT('Ctrl Pts',(-0.111486636987321,-0.101077771820372,
0.703796608422136));
#19955=CARTESIAN_POINT('Ctrl Pts',(0.02452690272786,-0.148473624679578,
0.711738776544918));
#19956=CARTESIAN_POINT('Ctrl Pts',(0.138071279799868,-0.0598523840572839,
0.719680944667696));
#19957=CARTESIAN_POINT('Ctrl Pts',(0.125128179973684,0.0835997892305201,
0.727623112790477));
#19958=CARTESIAN_POINT('Ctrl Pts',(-0.00244518761474098,0.150465967050502,
0.735565280913257));
#19959=CARTESIAN_POINT('Ctrl Pts',(-0.127778512144395,0.0794898610961098,
0.743507449036036));
#19960=CARTESIAN_POINT('Ctrl Pts',(-0.136053592364468,-0.0643071239260258,
0.751449617158818));
#19961=CARTESIAN_POINT('Ctrl Pts',(-0.019689604662082,-0.149192176910068,
0.759391785281597));
#19962=CARTESIAN_POINT('Ctrl Pts',(0.114712083700712,-0.0974018687498071,
0.767333953404378));
#19963=CARTESIAN_POINT('Ctrl Pts',(0.144025718573537,0.0436185576594447,
0.775276121527157));
#19964=CARTESIAN_POINT('Ctrl Pts',(0.0413969989087525,0.14467990414796,
0.783218289649938));
#19965=CARTESIAN_POINT('Ctrl Pts',(-0.0991556246317344,0.113199594905656,
0.791160457772717));
#19966=CARTESIAN_POINT('Ctrl Pts',(-0.148871509365196,-0.021983172706469,
0.799102625895497));
#19967=CARTESIAN_POINT('Ctrl Pts',(-0.062205797368885,-0.137027095702329,
0.807044794018277));
#19968=CARTESIAN_POINT('Ctrl Pts',(0.081446815661698,-0.126540121706451,
0.814986962141057));
#19969=CARTESIAN_POINT('Ctrl Pts',(0.150485778196879,-0.000129396266831759,
0.822929130263837));
#19970=CARTESIAN_POINT('Ctrl Pts',(0.0816643079123276,0.126399869446589,
0.830871298386618));
#19971=CARTESIAN_POINT('Ctrl Pts',(-0.0619700581130299,0.137133869194964,
0.838813466509397));
#19972=CARTESIAN_POINT('Ctrl Pts',(-0.148833484480893,0.0222391564630926,
0.846755634632177));
#19973=CARTESIAN_POINT('Ctrl Pts',(-0.0993501488194509,-0.113028908304323,
0.854697802754957));
#19974=CARTESIAN_POINT('Ctrl Pts',(0.041148129789194,-0.144750881164039,
0.862639970877736));
#19975=CARTESIAN_POINT('Ctrl Pts',(0.143950494202948,-0.0438661760544617,
0.870582139000517));
#19976=CARTESIAN_POINT('Ctrl Pts',(0.114879417330645,0.0972044528644933,
0.878524307123298));
#19977=CARTESIAN_POINT('Ctrl Pts',(-0.0194330078274841,0.149225816766708,
0.886466475246077));
#19978=CARTESIAN_POINT('Ctrl Pts',(-0.135942801386891,0.0645410019599824,
0.894408643368857));
#19979=CARTESIAN_POINT('Ctrl Pts',(-0.127915022941288,-0.0792700011911429,
0.902350811491637));
#19980=CARTESIAN_POINT('Ctrl Pts',(-0.00270394227186439,-0.150461539534541,
0.910292979614417));
#19981=CARTESIAN_POINT('Ctrl Pts',(0.124984227305131,-0.0838148501630433,
0.918235147737197));
#19982=CARTESIAN_POINT('Ctrl Pts',(0.138174004553101,0.0596148525845174,
0.926177315859977));
#19983=CARTESIAN_POINT('Ctrl Pts',(0.0247821984756025,0.148431225898158,
0.934119483982757));
#19984=CARTESIAN_POINT('Ctrl Pts',(-0.11131264737753,0.101269347369872,
0.942061652105537));
#19985=CARTESIAN_POINT('Ctrl Pts',(-0.145433672650089,-0.0386656571445607,
0.950003820228317));
#19986=CARTESIAN_POINT('Ctrl Pts',(-0.0463225128062989,-0.143178947440692,
0.957945988351097));
#19987=CARTESIAN_POINT('Ctrl Pts',(0.0952248276606132,-0.116525612549003,
0.965888156473877));
#19988=CARTESIAN_POINT('Ctrl Pts',(0.149536443172165,0.0168771545685866,
0.973830324596656));
#19989=CARTESIAN_POINT('Ctrl Pts',(0.0668573142755158,0.134818714245386,
0.981772492719438));
#19990=CARTESIAN_POINT('Ctrl Pts',(-0.0770699830103684,0.129252481220654,
0.989714660842216));
#19991=CARTESIAN_POINT('Ctrl Pts',(-0.15039325815857,0.00527769678589187,
0.997656828964997));
#19992=CARTESIAN_POINT('Ctrl Pts',(-0.0859408583470751,-0.123532000103139,
1.00559899708778));
#19993=CARTESIAN_POINT('Ctrl Pts',(0.0572421967501742,-0.139173693973137,
1.01354116521056));
#19994=CARTESIAN_POINT('Ctrl Pts',(0.147985518909957,-0.0273179863069172,
1.02148333333334));
#19995=CARTESIAN_POINT('Ctrl Pts',(0.103158902618224,0.109563803299803,
1.02942550145612));
#19996=CARTESIAN_POINT('Ctrl Pts',(-0.0361718663885326,0.146073893166727,
1.0373676695789));
#19997=CARTESIAN_POINT('Ctrl Pts',(-0.142365489706367,0.0487652901517079,
1.04530983770168));
#19998=CARTESIAN_POINT('Ctrl Pts',(-0.118137698690712,-0.0932173284908804,
1.05325200582446));
#19999=CARTESIAN_POINT('Ctrl Pts',(0.0143163610725534,-0.149803297655807,
1.06119417394724));
#20000=CARTESIAN_POINT('Ctrl Pts',(0.133655163317704,-0.0691540562905145,
1.06913634207002));
#20001=CARTESIAN_POINT('Ctrl Pts',(0.130552105047211,0.0748474051030229,
1.0770785101928));
#20002=CARTESIAN_POINT('Ctrl Pts',(0.0078499064261323,0.150280954056111,
1.08502067831558));
#20003=CARTESIAN_POINT('Ctrl Pts',(-0.122043612932812,0.0880417101447944,
1.09296284643836));
#20004=CARTESIAN_POINT('Ctrl Pts',(-0.140132644828567,-0.0548527851276936,
1.10090501456114));
#20005=CARTESIAN_POINT('Ctrl Pts',(-0.0298457776877653,-0.147496493982489,
1.10884718268392));
#20006=CARTESIAN_POINT('Ctrl Pts',(0.107782887988268,-0.10501826145877,
1.1167893508067));
#20007=CARTESIAN_POINT('Ctrl Pts',(0.146671355310253,0.033667487497105,
1.12473151892948));
#20008=CARTESIAN_POINT('Ctrl Pts',(0.0511937930472066,0.141510359113225,
1.13267368705226));
#20009=CARTESIAN_POINT('Ctrl Pts',(-0.0911825429852659,0.119715203870077,
1.14061585517504));
#20010=CARTESIAN_POINT('Ctrl Pts',(-0.150026302104679,-0.0117513769282424,
1.14855802329782));
#20011=CARTESIAN_POINT('Ctrl Pts',(-0.0714305557085884,-0.132452489195471,
1.1565001914206));
#20012=CARTESIAN_POINT('Ctrl Pts',(0.0726029180563751,-0.131813513998426,
1.16444235954338));
#20013=CARTESIAN_POINT('Ctrl Pts',(0.150124660100533,-0.010419818262018,
1.17238452766616));
#20014=CARTESIAN_POINT('Ctrl Pts',(0.0901167906002831,0.120519501471002,
1.18032669578894));
#20015=CARTESIAN_POINT('Ctrl Pts',(-0.0524473171394798,0.141050576417769,
1.18826886391172));
#20016=CARTESIAN_POINT('Ctrl Pts',(-0.146964294261872,0.0323648326895764,
1.1962110320345));
#20017=CARTESIAN_POINT('Ctrl Pts',(-0.106846879624786,-0.105970422747861,
1.20415320015727));
#20018=CARTESIAN_POINT('Ctrl Pts',(0.0311532535456026,-0.14722588419309,
1.21209536828006));
#20019=CARTESIAN_POINT('Ctrl Pts',(0.140613805972886,-0.0536073106276968,
1.22003753640283));
#20020=CARTESIAN_POINT('Ctrl Pts',(0.121257666323848,0.0891210667609394,
1.22797970452562));
#20021=CARTESIAN_POINT('Ctrl Pts',(-0.00918295295119051,0.150205391241489,
1.2359218726484));
#20022=CARTESIAN_POINT('Ctrl Pts',(-0.131211043922368,0.0736861461587066,
1.24386404077118));
#20023=CARTESIAN_POINT('Ctrl Pts',(-0.133036338837895,-0.0703371788708997,
1.25180620889396));
#20024=CARTESIAN_POINT('Ctrl Pts',(-0.0129866800356469,-0.149924422041766,
1.25974837701674));
#20025=CARTESIAN_POINT('Ctrl Pts',(0.118960111851797,-0.0921654923014072,
1.26769054513952));
#20026=CARTESIAN_POINT('Ctrl Pts',(0.141927220045961,0.050026496908035,
1.2756327132623));
#20027=CARTESIAN_POINT('Ctrl Pts',(0.0348744139414821,0.146389075532006,
1.28357488138508));
#20028=CARTESIAN_POINT('Ctrl Pts',(-0.104126938119509,0.108644221848311,
1.29151704950786));
#20029=CARTESIAN_POINT('Ctrl Pts',(-0.147737317493493,-0.0286299004949125,
1.29945921763064));
#20030=CARTESIAN_POINT('Ctrl Pts',(-0.0560051364173496,-0.139676092720537,
1.30740138575342));
#20031=CARTESIAN_POINT('Ctrl Pts',(0.0870335032532438,-0.122764634549313,
1.3153435538762));
#20032=CARTESIAN_POINT('Ctrl Pts',(0.150340512633584,0.00661184096937889,
1.32328572199898));
#20033=CARTESIAN_POINT('Ctrl Pts',(0.0759201674095095,0.129931190880528,
1.33122789012176));
#20034=CARTESIAN_POINT('Ctrl Pts',(-0.0680508508044829,0.134220221643466,
1.33917005824454));
#20035=CARTESIAN_POINT('Ctrl Pts',(-0.149680298423566,0.0155497403439283,
1.34711222636732));
#20036=CARTESIAN_POINT('Ctrl Pts',(-0.0941872156892785,-0.117365900463673,
1.3550543944901));
#20037=CARTESIAN_POINT('Ctrl Pts',(0.0475910332998192,-0.142762319241037,
1.36299656261288));
#20038=CARTESIAN_POINT('Ctrl Pts',(0.145771005694385,-0.0373737865856905,
1.37093873073566));
#20039=CARTESIAN_POINT('Ctrl Pts',(0.110409762917901,0.10225297323032,1.37888089885844));
#20040=CARTESIAN_POINT('Ctrl Pts',(-0.0260981686868614,0.148205506441964,
1.38682306698121));
#20041=CARTESIAN_POINT('Ctrl Pts',(-0.138697490589939,0.0583865667538053,
1.394765235104));
#20042=CARTESIAN_POINT('Ctrl Pts',(-0.124235673603468,-0.0849204601545819,
1.40270740322677));
#20043=CARTESIAN_POINT('Ctrl Pts',(0.0040388053119065,-0.150431633134115,
1.41064957134956));
#20044=CARTESIAN_POINT('Ctrl Pts',(0.12861328245382,-0.0781319533624403,
1.41859173947234));
#20045=CARTESIAN_POINT('Ctrl Pts',(0.1353648581188,0.0657445800149866,1.42653390759512));
#20046=CARTESIAN_POINT('Ctrl Pts',(0.0181081687242482,0.149392404544468,
1.43447607571789));
#20047=CARTESIAN_POINT('Ctrl Pts',(-0.115737181672069,0.0961812857364522,
1.44241824384068));
#20048=CARTESIAN_POINT('Ctrl Pts',(-0.143555918690644,-0.0451414811888502,
1.45036041196346));
#20049=CARTESIAN_POINT('Ctrl Pts',(-0.0398616700558823,-0.145110565703753,
1.45830258008624));
#20050=CARTESIAN_POINT('Ctrl Pts',(0.100348034367198,-0.112142416378873,
1.46624474820902));
#20051=CARTESIAN_POINT('Ctrl Pts',(0.14863229283285,0.0235577176564554,
1.4741869163318));
#20052=CARTESIAN_POINT('Ctrl Pts',(0.0607471474677608,0.137680339497592,
1.48212908445458));
#20053=CARTESIAN_POINT('Ctrl Pts',(-0.0827754224726193,0.125666453945577,
1.49007125257736));
#20054=CARTESIAN_POINT('Ctrl Pts',(-0.150492272191201,-0.00145719475437189,
1.49801342070014));
#20055=CARTESIAN_POINT('Ctrl Pts',(-0.0802951178786721,-0.12727177793954,
1.50595558882292));
#20056=CARTESIAN_POINT('Ctrl Pts',(0.0633700050447994,-0.136443062004882,
1.5138977569457));
#20057=CARTESIAN_POINT('Ctrl Pts',(0.149155357006591,-0.0207133070603065,
1.52183992506848));
#20058=CARTESIAN_POINT('Ctrl Pts',(0.0979555318420461,0.114182655252422,
1.52978209319126));
#20059=CARTESIAN_POINT('Ctrl Pts',(0.00450803278943675,0.134083974545181,
1.53507687193978));
#20060=CARTESIAN_POINT('Ctrl Pts',(-0.0361033354337414,0.122073089461022,
1.53772426131404));
#20061=CARTESIAN_POINT('Ctrl Pts',(-0.0592743564846203,0.123319225136773,
-0.00549926131403157));
#20062=CARTESIAN_POINT('Ctrl Pts',(-0.100300290071938,0.10359978715075,
-0.00285187193977157));
#20063=CARTESIAN_POINT('Ctrl Pts',(-0.160414584165772,0.0203416160441626,
0.00244290680874841));
#20064=CARTESIAN_POINT('Ctrl Pts',(-0.103922107946056,-0.124084444561314,
0.0103850749315284));
#20065=CARTESIAN_POINT('Ctrl Pts',(0.0479099321398382,-0.154436663180837,
0.0183272430543084));
#20066=CARTESIAN_POINT('Ctrl Pts',(0.155781551077148,-0.0435098515708298,
0.0262694111770884));
#20067=CARTESIAN_POINT('Ctrl Pts',(0.120977930992648,0.107381072623318,
0.0342115792998684));
#20068=CARTESIAN_POINT('Ctrl Pts',(-0.0246731903087699,0.159844935900913,
0.0421537474226484));
#20069=CARTESIAN_POINT('Ctrl Pts',(-0.147710978397823,0.0659033513787588,
0.0500959155454284));
#20070=CARTESIAN_POINT('Ctrl Pts',(-0.135435684249567,-0.0884277117007276,
0.0580380836682085));
#20071=CARTESIAN_POINT('Ctrl Pts',(0.000915427738408385,-0.16174188059703,
0.0659802517909884));
#20072=CARTESIAN_POINT('Ctrl Pts',(0.13642643003965,-0.0868880976295618,
0.0739224199137684));
#20073=CARTESIAN_POINT('Ctrl Pts',(0.146957588340267,0.0675663355536457,
0.0818645880365484));
#20074=CARTESIAN_POINT('Ctrl Pts',(0.0228600865593111,0.160121891352391,
0.0898067561593285));
#20075=CARTESIAN_POINT('Ctrl Pts',(-0.122179386207322,0.105989962368389,
0.0977489242821083));
#20076=CARTESIAN_POINT('Ctrl Pts',(-0.155290103436038,-0.0452399862206161,
0.105691092404888));
#20077=CARTESIAN_POINT('Ctrl Pts',(-0.0461390722131997,-0.155025288408554,
0.113633260527668));
#20078=CARTESIAN_POINT('Ctrl Pts',(0.105280057525145,-0.122791590307548,
0.121575428650448));
#20079=CARTESIAN_POINT('Ctrl Pts',(0.160251855424436,0.0219318669073289,
0.129517596773229));
#20080=CARTESIAN_POINT('Ctrl Pts',(0.0684164816681947,0.146563455853242,
0.137459764896008));
#20081=CARTESIAN_POINT('Ctrl Pts',(-0.086095413359615,0.136927875387926,
0.145401933018789));
#20082=CARTESIAN_POINT('Ctrl Pts',(-0.16173506727009,0.00185228698694943,
0.153344101141568));
#20083=CARTESIAN_POINT('Ctrl Pts',(-0.0892087826023274,-0.134920182928699,
0.161286269264348));
#20084=CARTESIAN_POINT('Ctrl Pts',(0.0650419110192955,-0.148091906331324,
0.169228437387128));
#20085=CARTESIAN_POINT('Ctrl Pts',(0.159707532494063,-0.025596228460074,
0.177170605509908));
#20086=CARTESIAN_POINT('Ctrl Pts',(0.108064646638443,0.120348223746572,
0.185112773632688));
#20087=CARTESIAN_POINT('Ctrl Pts',(-0.0425765573421325,0.156041339440091,
0.193054941755468));
#20088=CARTESIAN_POINT('Ctrl Pts',(-0.154213260793436,0.0487845573223287,
0.200997109878248));
#20089=CARTESIAN_POINT('Ctrl Pts',(-0.124574774400312,-0.103163891052585,
0.208939278001028));
#20090=CARTESIAN_POINT('Ctrl Pts',(0.0191870033818907,-0.160603616835255,
0.216881446123808));
#20091=CARTESIAN_POINT('Ctrl Pts',(0.145371514918136,-0.0709139301387177,
0.224823614246588));
#20092=CARTESIAN_POINT('Ctrl Pts',(0.138380784202201,0.0837402018183176,
0.232765782369368));
#20093=CARTESIAN_POINT('Ctrl Pts',(0.00461903876105218,0.161679705957985,
0.240707950492149));
#20094=CARTESIAN_POINT('Ctrl Pts',(-0.133374220718213,0.0915039894496894,
0.248650118614928));
#20095=CARTESIAN_POINT('Ctrl Pts',(-0.149182991964712,-0.0624987819548612,
0.256592286737709));
#20096=CARTESIAN_POINT('Ctrl Pts',(-0.0283248164207669,-0.159246248345813,
0.264534454860488));
#20097=CARTESIAN_POINT('Ctrl Pts',(0.118481800883715,-0.110107791262854,
0.272476622983269));
#20098=CARTESIAN_POINT('Ctrl Pts',(0.156746916480749,0.0399007144198201,
0.280418791106048));
#20099=CARTESIAN_POINT('Ctrl Pts',(0.0514157533588968,0.153356066537929,
0.288360959228829));
#20100=CARTESIAN_POINT('Ctrl Pts',(-0.101017521980764,0.126321506839912,
0.296303127351608));
#20101=CARTESIAN_POINT('Ctrl Pts',(-0.160908369261695,-0.0164365306249019,
0.304245295474388));
#20102=CARTESIAN_POINT('Ctrl Pts',(-0.0733906195540655,-0.144137017448375,
0.312187463597168));
#20103=CARTESIAN_POINT('Ctrl Pts',(0.0813604773699057,-0.13979318853071,
0.320129631719948));
#20104=CARTESIAN_POINT('Ctrl Pts',(0.161577018543625,-0.00738443741900211,
0.328071799842729));
#20105=CARTESIAN_POINT('Ctrl Pts',(0.0937724112935796,0.131789217000595,
0.336013967965508));
#20106=CARTESIAN_POINT('Ctrl Pts',(-0.0599373583072218,0.150230409426965,
0.343956136088289));
#20107=CARTESIAN_POINT('Ctrl Pts',(-0.158738350099833,0.0310451130618767,
0.351898304211068));
#20108=CARTESIAN_POINT('Ctrl Pts',(-0.112118705390683,-0.116580696253536,
0.359840472333849));
#20109=CARTESIAN_POINT('Ctrl Pts',(0.0372131918485748,-0.15740661101073,
0.367782640456628));
#20110=CARTESIAN_POINT('Ctrl Pts',(0.152453982298084,-0.0540318990865351,
0.375724808579408));
#20111=CARTESIAN_POINT('Ctrl Pts',(0.128031262769868,0.0988415833088236,
0.383666976702188));
#20112=CARTESIAN_POINT('Ctrl Pts',(-0.0136812466069205,0.161166021011634,
0.391609144824968));
#20113=CARTESIAN_POINT('Ctrl Pts',(-0.142860328563903,0.0758458262533652,
0.399551312947749));
#20114=CARTESIAN_POINT('Ctrl Pts',(-0.141164672957165,-0.0789569372907697,
0.407493481070528));
#20115=CARTESIAN_POINT('Ctrl Pts',(-0.0101476745237983,-0.161427034722196,
0.415435649193308));
#20116=CARTESIAN_POINT('Ctrl Pts',(0.130165636283581,-0.0960133843187101,
0.423377817316089));
#20117=CARTESIAN_POINT('Ctrl Pts',(0.151233851831306,0.0573583899504574,
0.431319985438868));
#20118=CARTESIAN_POINT('Ctrl Pts',(0.0337563222576384,0.158183986373718,
0.439262153561649));
#20119=CARTESIAN_POINT('Ctrl Pts',(-0.114645466422773,0.114096800420287,
0.447204321684428));
#20120=CARTESIAN_POINT('Ctrl Pts',(-0.158020229883659,-0.0345147763277912,
0.455146489807208));
#20121=CARTESIAN_POINT('Ctrl Pts',(-0.0566322287360923,-0.151507272121918,
0.463088657929988));
#20122=CARTESIAN_POINT('Ctrl Pts',(0.0966367119836487,-0.129703541718919,
0.471030826052768));
#20123=CARTESIAN_POINT('Ctrl Pts',(0.161376496659739,0.0109219578497271,
0.478972994175549));
#20124=CARTESIAN_POINT('Ctrl Pts',(0.0782788315581001,0.141541821972661,
0.486915162298328));
#20125=CARTESIAN_POINT('Ctrl Pts',(-0.0765302851406724,0.142494836024782,
0.494857330421108));
#20126=CARTESIAN_POINT('Ctrl Pts',(-0.161229798395673,0.0129079412274925,
0.502799498543889));
#20127=CARTESIAN_POINT('Ctrl Pts',(-0.0982262525537151,-0.128503953817366,
0.510741666666668));
#20128=CARTESIAN_POINT('Ctrl Pts',(0.0547626317937811,-0.152193025452748,
0.518683834789449));
#20129=CARTESIAN_POINT('Ctrl Pts',(0.157583319439253,-0.0364576503898468,
0.526626002912228));
#20130=CARTESIAN_POINT('Ctrl Pts',(0.116041497328862,0.112676677866884,
0.534568171035008));
#20131=CARTESIAN_POINT('Ctrl Pts',(-0.0318062577307366,0.158587593482618,
0.542510339157789));
#20132=CARTESIAN_POINT('Ctrl Pts',(-0.150516213127973,0.0592159811457737,
0.550452507280567));
#20133=CARTESIAN_POINT('Ctrl Pts',(-0.131337854181896,-0.0944035534094825,
0.558394675403349));
#20134=CARTESIAN_POINT('Ctrl Pts',(0.00815947204521347,-0.161539734596121,
0.566336843526128));
#20135=CARTESIAN_POINT('Ctrl Pts',(0.140181883624494,-0.080688923285235,
0.574279011648909));
#20136=CARTESIAN_POINT('Ctrl Pts',(0.143783288371658,0.0740812312429708,
0.582221179771688));
#20137=CARTESIAN_POINT('Ctrl Pts',(0.0156644295519346,0.160985367298567,
0.590163347894469));
#20138=CARTESIAN_POINT('Ctrl Pts',(-0.126804656005353,0.100410368253513,
0.598105516017247));
#20139=CARTESIAN_POINT('Ctrl Pts',(-0.153107649524464,-0.0521508436608248,
0.606047684140029));
#20140=CARTESIAN_POINT('Ctrl Pts',(-0.0391483067326994,-0.156936525122116,
0.613989852262808));
#20141=CARTESIAN_POINT('Ctrl Pts',(0.110674906884577,-0.117952226869747,
0.621932020385589));
#20142=CARTESIAN_POINT('Ctrl Pts',(0.159108535730396,0.0290884288879846,
0.629874188508368));
#20143=CARTESIAN_POINT('Ctrl Pts',(0.061782400006242,0.14948109541648,0.637816356631148));
#20144=CARTESIAN_POINT('Ctrl Pts',(-0.0921427612707386,0.132933721767072,
0.645758524753929));
#20145=CARTESIAN_POINT('Ctrl Pts',(-0.161655687038194,-0.0053945978210935,
0.653700692876707));
#20146=CARTESIAN_POINT('Ctrl Pts',(-0.0830753959589387,-0.138780911597048,
0.661642860999489));
#20147=CARTESIAN_POINT('Ctrl Pts',(0.0716104924784035,-0.145029652845349,
0.669585029122267));
#20148=CARTESIAN_POINT('Ctrl Pts',(0.160693812980115,-0.0184163326249747,
0.677527197245049));
#20149=CARTESIAN_POINT('Ctrl Pts',(0.102565092089392,0.125068240261613,
0.685469365367828));
#20150=CARTESIAN_POINT('Ctrl Pts',(-0.0495237900674707,0.153977456320057,
0.693411533490608));
#20151=CARTESIAN_POINT('Ctrl Pts',(-0.156243792750268,0.0418275036842162,
0.701353701613389));
#20152=CARTESIAN_POINT('Ctrl Pts',(-0.119828429739121,-0.108640739429086,
0.709295869736167));
#20153=CARTESIAN_POINT('Ctrl Pts',(0.0263620853553792,-0.159582904138124,
0.717238037858949));
#20154=CARTESIAN_POINT('Ctrl Pts',(0.148402221984423,-0.0643307340819919,
0.725180205981728));
#20155=CARTESIAN_POINT('Ctrl Pts',(0.134490677336207,0.0898549973406614,
0.733122374104509));
#20156=CARTESIAN_POINT('Ctrl Pts',(-0.00262814450422035,0.161724320044658,
0.741064542227287));
#20157=CARTESIAN_POINT('Ctrl Pts',(-0.137339315979238,0.0854375510170853,
0.749006710350069));
#20158=CARTESIAN_POINT('Ctrl Pts',(-0.146233564613262,-0.0691187920752458,
0.756948878472847));
#20159=CARTESIAN_POINT('Ctrl Pts',(-0.0211628449166461,-0.160355220783347,
0.764891046595629));
#20160=CARTESIAN_POINT('Ctrl Pts',(0.12329521486528,-0.104689793336152,
0.772833214718408));
#20161=CARTESIAN_POINT('Ctrl Pts',(0.154802191231926,0.0468822399980663,
0.780775382841188));
#20162=CARTESIAN_POINT('Ctrl Pts',(0.0444944569967772,0.155505325098544,
0.788717550963968));
#20163=CARTESIAN_POINT('Ctrl Pts',(-0.106574770936664,0.121669556739719,
0.796659719086747));
#20164=CARTESIAN_POINT('Ctrl Pts',(-0.160010559849905,-0.0236280251811701,
0.804601887209529));
#20165=CARTESIAN_POINT('Ctrl Pts',(-0.0668602374312443,-0.147279908636853,
0.812544055332307));
#20166=CARTESIAN_POINT('Ctrl Pts',(0.0875409312876049,-0.13600826514128,
0.820486223455089));
#20167=CARTESIAN_POINT('Ctrl Pts',(0.161745613525436,-0.000139078116330951,
0.828428391577867));
#20168=CARTESIAN_POINT('Ctrl Pts',(0.0877746970157421,0.135857518751215,
0.836370559700649));
#20169=CARTESIAN_POINT('Ctrl Pts',(-0.0666068593976089,0.147394671269449,
0.844312727823428));
#20170=CARTESIAN_POINT('Ctrl Pts',(-0.159969689820096,0.0239031624749592,
0.852254895946208));
#20171=CARTESIAN_POINT('Ctrl Pts',(-0.106783850056725,-0.121486098811777,
0.860197064068988));
#20172=CARTESIAN_POINT('Ctrl Pts',(0.0442269666803361,-0.155581612845794,
0.868139232191768));
#20173=CARTESIAN_POINT('Ctrl Pts',(0.154721338329289,-0.0471483860066884,
0.876081400314548));
#20174=CARTESIAN_POINT('Ctrl Pts',(0.123475068941597,0.104477606152275,
0.884023568437328));
#20175=CARTESIAN_POINT('Ctrl Pts',(-0.0208870486723946,0.160391377683462,
0.891965736560109));
#20176=CARTESIAN_POINT('Ctrl Pts',(-0.146114483894434,0.0693701696243073,
0.899907904682887));
#20177=CARTESIAN_POINT('Ctrl Pts',(-0.137486040957907,-0.0852012404790134,
0.907850072805669));
#20178=CARTESIAN_POINT('Ctrl Pts',(-0.00290626002629624,-0.161719561247554,
0.915792240928448));
#20179=CARTESIAN_POINT('Ctrl Pts',(0.134335953660838,-0.0900861498315643,
0.923734409051229));
#20180=CARTESIAN_POINT('Ctrl Pts',(0.148512632937768,0.0640754297319473,
0.931676577174007));
#20181=CARTESIAN_POINT('Ctrl Pts',(0.0266364831612253,0.159537332941991,
0.939618745296788));
#20182=CARTESIAN_POINT('Ctrl Pts',(-0.119641421660886,0.10884664928423,
0.947560913419568));
#20183=CARTESIAN_POINT('Ctrl Pts',(-0.156315493011378,-0.0415587473590326,
0.955503081542348));
#20184=CARTESIAN_POINT('Ctrl Pts',(-0.0497885138626987,-0.153892061929087,
0.963445249665127));
#20185=CARTESIAN_POINT('Ctrl Pts',(0.102349858952582,-0.125244437839883,
0.971387417787908));
#20186=CARTESIAN_POINT('Ctrl Pts',(0.160725246166783,0.018139958160622,
0.979329585910688));
#20187=CARTESIAN_POINT('Ctrl Pts',(0.0718597959603077,0.14490628889729,
0.987271754033468));
#20188=CARTESIAN_POINT('Ctrl Pts',(-0.0828366097831417,0.138923572215364,
0.995213922156248));
#20189=CARTESIAN_POINT('Ctrl Pts',(-0.161646170836971,0.00567259122332548,
1.00315609027903));
#20190=CARTESIAN_POINT('Ctrl Pts',(-0.0923712328620446,-0.132775066096718,
1.01109825840181));
#20191=CARTESIAN_POINT('Ctrl Pts',(0.0615252440718216,-0.149587122371362,
1.01904042652459));
#20192=CARTESIAN_POINT('Ctrl Pts',(0.159058276707423,-0.0293620068848675,
1.02698259464737));
#20193=CARTESIAN_POINT('Ctrl Pts',(0.1108775872014,0.117761723381742,1.03492476277015));
#20194=CARTESIAN_POINT('Ctrl Pts',(-0.0388783630684312,0.157003616909169,
1.04286693089293));
#20195=CARTESIAN_POINT('Ctrl Pts',(-0.153017738641585,0.0524140677533946,
1.05080909901571));
#20196=CARTESIAN_POINT('Ctrl Pts',(-0.126977145509477,-0.10019215216626,
1.05875126713849));
#20197=CARTESIAN_POINT('Ctrl Pts',(0.0153875577671049,-0.161012067570745,
1.06669343526127));
#20198=CARTESIAN_POINT('Ctrl Pts',(0.143655677305146,-0.0743283876822416,
1.07463560338405));
#20199=CARTESIAN_POINT('Ctrl Pts',(0.140320438123209,0.080447731368589,
1.08257777150683));
#20200=CARTESIAN_POINT('Ctrl Pts',(0.00843726195408678,0.161525463776335,
1.09051993962961));
#20201=CARTESIAN_POINT('Ctrl Pts',(-0.131175312957834,0.094629277223576,
1.09846210775239));
#20202=CARTESIAN_POINT('Ctrl Pts',(-0.150617825048456,-0.0589570489009974,
1.10640427587517));
#20203=CARTESIAN_POINT('Ctrl Pts',(-0.0320789358376135,-0.158532661344495,
1.11434644399795));
#20204=CARTESIAN_POINT('Ctrl Pts',(0.115847554194776,-0.112876069317329,
1.12228861212073));
#20205=CARTESIAN_POINT('Ctrl Pts',(0.157645783113317,0.0361865984037055,
1.13023078024351));
#20206=CARTESIAN_POINT('Ctrl Pts',(0.0550242791334153,0.152098624396442,
1.13817294836629));
#20207=CARTESIAN_POINT('Ctrl Pts',(-0.0980051173916675,0.128672684756662,
1.14611511648907));
#20208=CARTESIAN_POINT('Ctrl Pts',(-0.161251757937727,-0.0126306531673768,
1.15405728461185));
#20209=CARTESIAN_POINT('Ctrl Pts',(-0.0767752221903169,-0.142363015193798,
1.16199945273463));
#20210=CARTESIAN_POINT('Ctrl Pts',(0.0780353045016797,-0.141676229794458,
1.16994162085741));
#20211=CARTESIAN_POINT('Ctrl Pts',(0.161357475398708,-0.0111994629512984,
1.17788378898019));
#20212=CARTESIAN_POINT('Ctrl Pts',(0.0968596219472387,0.129537162519796,
1.18582595710297));
#20213=CARTESIAN_POINT('Ctrl Pts',(-0.0563715959749383,0.151604439264423,
1.19376812522575));
#20214=CARTESIAN_POINT('Ctrl Pts',(-0.157960640709981,0.0347864747270306,
1.20171029334853));
#20215=CARTESIAN_POINT('Ctrl Pts',(-0.114841510641486,-0.113899474410655,
1.20965246147131));
#20216=CARTESIAN_POINT('Ctrl Pts',(0.03348424129126,-0.158241803650584,
1.21759462959409));
#20217=CARTESIAN_POINT('Ctrl Pts',(0.151134988234409,-0.0576183839484237,
1.22553679771687));
#20218=CARTESIAN_POINT('Ctrl Pts',(0.130330559267559,0.0957893948119858,
1.23347896583965));
#20219=CARTESIAN_POINT('Ctrl Pts',(-0.0098700513554357,0.16144424710618,
1.24142113396243));
#20220=CARTESIAN_POINT('Ctrl Pts',(-0.141028680947982,0.0791995832534545,
1.24936330208521));
#20221=CARTESIAN_POINT('Ctrl Pts',(-0.142990550365238,-0.0756000353418,
1.25730547020799));
#20222=CARTESIAN_POINT('Ctrl Pts',(-0.013958385670676,-0.161142254877177,
1.26524763833077));
#20223=CARTESIAN_POINT('Ctrl Pts',(0.127861094297897,-0.0990616141723472,
1.27318980645355));
#20224=CARTESIAN_POINT('Ctrl Pts',(0.152546676219863,0.0537696421008814,
1.28113197457633));
#20225=CARTESIAN_POINT('Ctrl Pts',(0.0374838310097642,0.157342382244044,
1.28907414269911));
#20226=CARTESIAN_POINT('Ctrl Pts',(-0.111918054267102,0.116773335855419,
1.29701631082189));
#20227=CARTESIAN_POINT('Ctrl Pts',(-0.158791504053787,-0.0307720827589687,
1.30495847894467));
#20228=CARTESIAN_POINT('Ctrl Pts',(-0.060195622861772,-0.150127112226926,
1.31290064706745));
#20229=CARTESIAN_POINT('Ctrl Pts',(0.0935456330135535,-0.131950283756556,
1.32084281519023));
#20230=CARTESIAN_POINT('Ctrl Pts',(0.161589478720268,0.00710656041347678,
1.32878498331301));
#20231=CARTESIAN_POINT('Ctrl Pts',(0.0816007612396376,0.139653065139265,
1.33672715143579));
#20232=CARTESIAN_POINT('Ctrl Pts',(-0.0731426367739486,0.144263015132499,
1.34466931955857));
#20233=CARTESIAN_POINT('Ctrl Pts',(-0.160879865135934,0.0167132224867059,
1.35261148768135));
#20234=CARTESIAN_POINT('Ctrl Pts',(-0.101234609479067,-0.126147598829082,
1.36055365580413));
#20235=CARTESIAN_POINT('Ctrl Pts',(0.051151949184981,-0.153444260252591,
1.36849582392691));
#20236=CARTESIAN_POINT('Ctrl Pts',(0.15667806641111,-0.0401702148435725,
1.37643799204969));
#20237=CARTESIAN_POINT('Ctrl Pts',(0.118670980449659,0.10990387323047,1.38438016017247));
#20238=CARTESIAN_POINT('Ctrl Pts',(-0.0280509185434417,0.159294724422008,
1.39232232829525));
#20239=CARTESIAN_POINT('Ctrl Pts',(-0.149075287902345,0.0627552395607943,
1.40026449641803));
#20240=CARTESIAN_POINT('Ctrl Pts',(-0.133531390736797,-0.0912744851582948,
1.40820666454081));
#20241=CARTESIAN_POINT('Ctrl Pts',(0.00434100186018791,-0.161687417152987,
1.41614883266359));
#20242=CARTESIAN_POINT('Ctrl Pts',(0.138236546518021,-0.0839780402106489,
1.42409100078637));
#20243=CARTESIAN_POINT('Ctrl Pts',(0.145493297031458,0.07066380330362,1.43203316890915));
#20244=CARTESIAN_POINT('Ctrl Pts',(0.0194630807988606,0.160570430100525,
1.43997533703193));
#20245=CARTESIAN_POINT('Ctrl Pts',(-0.124397014000637,0.103377882332206,
1.44791750515471));
#20246=CARTESIAN_POINT('Ctrl Pts',(-0.15429723939393,-0.0485191136187331,
1.45585967327749));
#20247=CARTESIAN_POINT('Ctrl Pts',(-0.042844249846,-0.155968210152522,1.46380184140027));
#20248=CARTESIAN_POINT('Ctrl Pts',(0.107856400646442,-0.120533276677448,
1.47174400952305));
#20249=CARTESIAN_POINT('Ctrl Pts',(0.159753444358638,0.0253203827049868,
1.47968617764583));
#20250=CARTESIAN_POINT('Ctrl Pts',(0.0652924466007548,0.147982030257331,
1.48762834576861));
#20251=CARTESIAN_POINT('Ctrl Pts',(-0.0889689487809616,0.13506922671723,
1.49557051389139));
#20252=CARTESIAN_POINT('Ctrl Pts',(-0.161752593421533,-0.00156622680492735,
1.50351268201417));
#20253=CARTESIAN_POINT('Ctrl Pts',(-0.086303059730943,-0.136794666273195,
1.51145485013695));
#20254=CARTESIAN_POINT('Ctrl Pts',(0.0681115549116652,-0.14665217563879,
1.51939701825973));
#20255=CARTESIAN_POINT('Ctrl Pts',(0.160315645894948,-0.02226314405755,
1.52733918638251));
#20256=CARTESIAN_POINT('Ctrl Pts',(0.105284883301553,0.122726172858702,
1.53528135450529));
#20257=CARTESIAN_POINT('Ctrl Pts',(0.00484533846358528,0.144116573583224,
1.54057613325381));
#20258=CARTESIAN_POINT('Ctrl Pts',(-0.0388047044047284,0.131206995015745,
1.54322352262807));
#20259=CARTESIAN_POINT('Ctrl Pts',(-0.0634007094575145,0.131904027763688,
-3.88578058618805E-16));
#20260=CARTESIAN_POINT('Ctrl Pts',(-0.107282641710421,0.110811831533068,
0.00264738937425961));
#20261=CARTESIAN_POINT('Ctrl Pts',(-0.171581760589518,0.0217576868851663,
0.0079421681227796));
#20262=CARTESIAN_POINT('Ctrl Pts',(-0.111156590520044,-0.1327225175337,
0.0158843362455596));
#20263=CARTESIAN_POINT('Ctrl Pts',(0.0512451567233008,-0.165187689797298,
0.0238265043683396));
#20264=CARTESIAN_POINT('Ctrl Pts',(0.16662620135312,-0.0465387668729445,
0.0317686724911196));
#20265=CARTESIAN_POINT('Ctrl Pts',(0.129399745666171,0.114856349193662,
0.0397108406138996));
#20266=CARTESIAN_POINT('Ctrl Pts',(-0.026390801400978,0.170972456562021,
0.0476530087366796));
#20267=CARTESIAN_POINT('Ctrl Pts',(-0.157993800025737,0.070491178324729,
0.0555951768594596));
#20268=CARTESIAN_POINT('Ctrl Pts',(-0.144863967768493,-0.0945835600760224,
0.0635373449822396));
#20269=CARTESIAN_POINT('Ctrl Pts',(0.000979154756195248,-0.17300145605975,
0.0714795131050195));
#20270=CARTESIAN_POINT('Ctrl Pts',(0.145923683802689,-0.0929367665856833,
0.0794216812277997));
#20271=CARTESIAN_POINT('Ctrl Pts',(0.157187963117837,0.0722699302633024,
0.0873638493505794));
#20272=CARTESIAN_POINT('Ctrl Pts',(0.0244514793930555,0.171268692120756,
0.0953060174733598));
#20273=CARTESIAN_POINT('Ctrl Pts',(-0.130684839550095,0.113368397534175,
0.103248185596139));
#20274=CARTESIAN_POINT('Ctrl Pts',(-0.166100541844429,-0.0483893439312075,
0.11119035371892));
#20275=CARTESIAN_POINT('Ctrl Pts',(-0.0493510193195793,-0.165817291858885,
0.119132521841699));
#20276=CARTESIAN_POINT('Ctrl Pts',(0.112609073040783,-0.131339661914923,
0.12707468996448));
#20277=CARTESIAN_POINT('Ctrl Pts',(0.17140770357293,0.0234586422209967,
0.135016858087259));
#20278=CARTESIAN_POINT('Ctrl Pts',(0.0731792588499177,0.156766393306209,
0.14295902621004));
#20279=CARTESIAN_POINT('Ctrl Pts',(-0.0920889000195865,0.146460037003638,
0.150901194332819));
#20280=CARTESIAN_POINT('Ctrl Pts',(-0.172994168426659,0.00198123296575728,
0.1588433624556));
#20281=CARTESIAN_POINT('Ctrl Pts',(-0.0954190048152776,-0.144312580095855,
0.16678553057838));
#20282=CARTESIAN_POINT('Ctrl Pts',(0.0695697692503139,-0.158401246055831,
0.17472769870116));
#20283=CARTESIAN_POINT('Ctrl Pts',(0.170825487889685,-0.0273780963649298,
0.18266986682394));
#20284=CARTESIAN_POINT('Ctrl Pts',(0.115587509852263,0.128726201683253,
0.19061203494672));
#20285=CARTESIAN_POINT('Ctrl Pts',(-0.0455405018601966,0.16690407474553,
0.198554203069499));
#20286=CARTESIAN_POINT('Ctrl Pts',(-0.164948735370872,0.0521806684752238,
0.20649637119228));
#20287=CARTESIAN_POINT('Ctrl Pts',(-0.133246981425072,-0.110345590758605,
0.214438539315059));
#20288=CARTESIAN_POINT('Ctrl Pts',(0.0205226964731592,-0.171783952668295,
0.22238070743784));
#20289=CARTESIAN_POINT('Ctrl Pts',(0.155491476033395,-0.0758505658746651,
0.230322875560619));
#20290=CARTESIAN_POINT('Ctrl Pts',(0.148014089296488,0.0895697316726553,
0.2382650436834));
#20291=CARTESIAN_POINT('Ctrl Pts',(0.00494059070111224,0.172934953166096,
0.24620721180618));
#20292=CARTESIAN_POINT('Ctrl Pts',(-0.142658996543838,0.0978739912732451,
0.25414937992896));
#20293=CARTESIAN_POINT('Ctrl Pts',(-0.159568287038446,-0.0668496016012732,
0.262091548051739));
#20294=CARTESIAN_POINT('Ctrl Pts',(-0.0302966335331915,-0.170332091689456,
0.27003371617452));
#20295=CARTESIAN_POINT('Ctrl Pts',(0.126729848780061,-0.11777288690896,
0.2779758842973));
#20296=CARTESIAN_POINT('Ctrl Pts',(0.167658770158652,0.0426783815482623,
0.28591805242008));
#20297=CARTESIAN_POINT('Ctrl Pts',(0.0549950338320791,0.164031867990689,
0.293860220542859));
#20298=CARTESIAN_POINT('Ctrl Pts',(-0.108049803339193,0.135115311719503,
0.30180238866564));
#20299=CARTESIAN_POINT('Ctrl Pts',(-0.1721099202737,-0.0175807510100837,
0.309744556788419));
#20300=CARTESIAN_POINT('Ctrl Pts',(-0.0784996687135917,-0.154171039675278,
0.3176867249112));
#20301=CARTESIAN_POINT('Ctrl Pts',(0.087024343965547,-0.14952481740522,
0.325628893033979));
#20302=CARTESIAN_POINT('Ctrl Pts',(0.172825117221703,-0.00789850112384905,
0.33357106115676));
#20303=CARTESIAN_POINT('Ctrl Pts',(0.100300328103893,0.140963653630822,
0.341513229279539));
#20304=CARTESIAN_POINT('Ctrl Pts',(-0.0641098658012952,0.160688619913292,
0.349455397402319));
#20305=CARTESIAN_POINT('Ctrl Pts',(-0.16978883637574,0.033206302186043,
0.357397565525099));
#20306=CARTESIAN_POINT('Ctrl Pts',(-0.119923789760104,-0.124696399756661,
0.36533973364788));
#20307=CARTESIAN_POINT('Ctrl Pts',(0.0398037685148125,-0.168364388974385,
0.373281901770659));
#20308=CARTESIAN_POINT('Ctrl Pts',(0.163066985633654,-0.0577933011607096,
0.38122406989344));
#20309=CARTESIAN_POINT('Ctrl Pts',(0.136944091404129,0.10572238784759,0.38916623801622));
#20310=CARTESIAN_POINT('Ctrl Pts',(-0.0146336593526265,0.172385508313924,
0.397108406138999));
#20311=CARTESIAN_POINT('Ctrl Pts',(-0.152805474769431,0.0811257933285562,
0.40505057426178));
#20312=CARTESIAN_POINT('Ctrl Pts',(-0.150991776994562,-0.0844534827151793,
0.412992742384559));
#20313=CARTESIAN_POINT('Ctrl Pts',(-0.0108540995180527,-0.172664692355881,
0.42093491050734));
#20314=CARTESIAN_POINT('Ctrl Pts',(0.139227048201004,-0.102697305280782,
0.428877078630119));
#20315=CARTESIAN_POINT('Ctrl Pts',(0.16176191642983,0.0613513639265466,
0.4368192467529));
#20316=CARTESIAN_POINT('Ctrl Pts',(0.0361062507758455,0.169195880912067,
0.444761414875679));
#20317=CARTESIAN_POINT('Ctrl Pts',(-0.12262644992489,0.12203958882886,0.45270358299846));
#20318=CARTESIAN_POINT('Ctrl Pts',(-0.169020724600573,-0.0369175042249048,
0.460645751121239));
#20319=CARTESIAN_POINT('Ctrl Pts',(-0.0605746513833496,-0.162054370729346,
0.468587919244019));
#20320=CARTESIAN_POINT('Ctrl Pts',(0.103364025571403,-0.138732785167649,
0.4765300873668));
#20321=CARTESIAN_POINT('Ctrl Pts',(0.172610636112938,0.0116822841681558,
0.484472255489579));
#20322=CARTESIAN_POINT('Ctrl Pts',(0.083728171010617,0.151395181039277,
0.49241442361236));
#20323=CARTESIAN_POINT('Ctrl Pts',(-0.081857900459256,0.152414538660527,
0.500356591735139));
#20324=CARTESIAN_POINT('Ctrl Pts',(-0.172453725526818,0.0138065207282529,
0.50829875985792));
#20325=CARTESIAN_POINT('Ctrl Pts',(-0.105064221167447,-0.137449688588867,
0.516240927980699));
#20326=CARTESIAN_POINT('Ctrl Pts',(0.0585749034388466,-0.162787862415564,
0.52418309610348));
#20327=CARTESIAN_POINT('Ctrl Pts',(0.168553398866689,-0.0389956304370821,
0.532125264226259));
#20328=CARTESIAN_POINT('Ctrl Pts',(0.124119664784058,0.120520605195094,
0.54006743234904));
#20329=CARTESIAN_POINT('Ctrl Pts',(-0.0340204335384149,0.16962758491636,
0.548009600471819));
#20330=CARTESIAN_POINT('Ctrl Pts',(-0.160994319687769,0.0633382703503284,
0.5559517685946));
#20331=CARTESIAN_POINT('Ctrl Pts',(-0.14048086942825,-0.100975406844349,
0.563893936717379));
#20332=CARTESIAN_POINT('Ctrl Pts',(0.00872748937560605,-0.172785237771916,
0.57183610484016));
#20333=CARTESIAN_POINT('Ctrl Pts',(0.149940571302356,-0.0863060399984934,
0.579778272962939));
#20334=CARTESIAN_POINT('Ctrl Pts',(0.153792685935992,0.0792383569699183,
0.58772044108572));
#20335=CARTESIAN_POINT('Ctrl Pts',(0.0167549005293281,0.17219227848818,
0.595662609208499));
#20336=CARTESIAN_POINT('Ctrl Pts',(-0.135632095058532,0.107400382926376,
0.60360477733128));
#20337=CARTESIAN_POINT('Ctrl Pts',(-0.163766157558233,-0.0557812970565469,
0.611546945454059));
#20338=CARTESIAN_POINT('Ctrl Pts',(-0.0418735953979919,-0.167861578305293,
0.61948911357684));
#20339=CARTESIAN_POINT('Ctrl Pts',(0.118379481984711,-0.126163408751231,
0.627431281699619));
#20340=CARTESIAN_POINT('Ctrl Pts',(0.17018479228316,0.0311134044783985,
0.6353734498224));
#20341=CARTESIAN_POINT('Ctrl Pts',(0.0660833491022344,0.159887142804326,
0.643315617945179));
#20342=CARTESIAN_POINT('Ctrl Pts',(-0.0985572308567358,0.142187832491218,
0.651257786067961));
#20343=CARTESIAN_POINT('Ctrl Pts',(-0.172909262181909,-0.00577013989488307,
0.659199954190738));
#20344=CARTESIAN_POINT('Ctrl Pts',(-0.0888586457050277,-0.148442071348278,
0.667142122313521));
#20345=CARTESIAN_POINT('Ctrl Pts',(0.0765956190331784,-0.155125815413241,
0.675084290436298));
#20346=CARTESIAN_POINT('Ctrl Pts',(0.171880427770071,-0.0196983758791502,
0.683026458559081));
#20347=CARTESIAN_POINT('Ctrl Pts',(0.109705106722326,0.133774799651286,
0.690968626681858));
#20348=CARTESIAN_POINT('Ctrl Pts',(-0.0529713625168984,0.164696515493808,
0.698910794804641));
#20349=CARTESIAN_POINT('Ctrl Pts',(-0.167120621735807,0.0447393032280997,
0.706852962927418));
#20350=CARTESIAN_POINT('Ctrl Pts',(-0.12817022249092,-0.116203707037801,
0.7147951310502));
#20351=CARTESIAN_POINT('Ctrl Pts',(0.0281972679828983,-0.17069218359667,
0.722737299172979));
#20352=CARTESIAN_POINT('Ctrl Pts',(0.158733164168978,-0.0688090841067,0.73067946729576));
#20353=CARTESIAN_POINT('Ctrl Pts',(0.14385317469873,0.0961102054508026,
0.738621635418538));
#20354=CARTESIAN_POINT('Ctrl Pts',(-0.00281110139369983,0.172982673038814,
0.746563803541321));
#20355=CARTESIAN_POINT('Ctrl Pts',(-0.146900119814081,0.0913852409380608,
0.754505971664098));
#20356=CARTESIAN_POINT('Ctrl Pts',(-0.156413536862055,-0.0739304602244656,
0.762448139786881));
#20357=CARTESIAN_POINT('Ctrl Pts',(-0.0226360851712103,-0.171518264656626,
0.770390307909658));
#20358=CARTESIAN_POINT('Ctrl Pts',(0.131878346029848,-0.111977717922496,
0.778332476032441));
#20359=CARTESIAN_POINT('Ctrl Pts',(0.165578663890314,0.0501459223366878,
0.786274644155218));
#20360=CARTESIAN_POINT('Ctrl Pts',(0.047591915084802,0.166330746049129,
0.794216812278001));
#20361=CARTESIAN_POINT('Ctrl Pts',(-0.113993917241593,0.130139518573781,
0.802158980400778));
#20362=CARTESIAN_POINT('Ctrl Pts',(-0.171149610334614,-0.0252728776558711,
0.81010114852356));
#20363=CARTESIAN_POINT('Ctrl Pts',(-0.0715146774936035,-0.157532721571376,
0.818043316646339));
#20364=CARTESIAN_POINT('Ctrl Pts',(0.0936350469135118,-0.14547640857611,
0.825985484769119));
#20365=CARTESIAN_POINT('Ctrl Pts',(0.173005448853992,-0.000148759965830227,
0.8339276528919));
#20366=CARTESIAN_POINT('Ctrl Pts',(0.0938850861191564,0.145315168055841,
0.841869821014678));
#20367=CARTESIAN_POINT('Ctrl Pts',(-0.0712436606821878,0.157655473343934,
0.849811989137461));
#20368=CARTESIAN_POINT('Ctrl Pts',(-0.171105895159299,0.0255671684868261,
0.857754157260238));
#20369=CARTESIAN_POINT('Ctrl Pts',(-0.114217551294,-0.129943289319231,0.86569632538302));
#20370=CARTESIAN_POINT('Ctrl Pts',(0.0473058035714782,-0.166412344527548,
0.873638493505798));
#20371=CARTESIAN_POINT('Ctrl Pts',(0.16549218245563,-0.0504305959589149,
0.88158066162858));
#20372=CARTESIAN_POINT('Ctrl Pts',(0.132070720552549,0.111750759440056,
0.889522829751358));
#20373=CARTESIAN_POINT('Ctrl Pts',(-0.022341089517305,0.171556938600217,
0.89746499787414));
#20374=CARTESIAN_POINT('Ctrl Pts',(-0.156286166401977,0.074199337288632,
0.905407165996919));
#20375=CARTESIAN_POINT('Ctrl Pts',(-0.147057058974526,-0.0911324797668838,
0.913349334119699));
#20376=CARTESIAN_POINT('Ctrl Pts',(-0.00310857778072832,-0.172977582960567,
0.92129150224248));
#20377=CARTESIAN_POINT('Ctrl Pts',(0.143687680016546,-0.0963574495000853,
0.929233670365259));
#20378=CARTESIAN_POINT('Ctrl Pts',(0.158851261322436,0.0685360068793772,
0.93717583848804));
#20379=CARTESIAN_POINT('Ctrl Pts',(0.0284907678468484,0.170643439985825,
0.945118006610819));
#20380=CARTESIAN_POINT('Ctrl Pts',(-0.127970195944242,0.116423951198588,
0.9530601747336));
#20381=CARTESIAN_POINT('Ctrl Pts',(-0.167197313372666,-0.0444518375735043,
0.961002342856378));
#20382=CARTESIAN_POINT('Ctrl Pts',(-0.0532545149190986,-0.164605176417482,
0.96894451097916));
#20383=CARTESIAN_POINT('Ctrl Pts',(0.10947489024455,-0.133963263130763,
0.976886679101939));
#20384=CARTESIAN_POINT('Ctrl Pts',(0.1719140491614,0.0194027617526574,0.984828847224719));
#20385=CARTESIAN_POINT('Ctrl Pts',(0.0768622776450996,0.154993863549195,
0.992771015347499));
#20386=CARTESIAN_POINT('Ctrl Pts',(-0.088603236555915,0.148594663210074,
1.00071318347028));
#20387=CARTESIAN_POINT('Ctrl Pts',(-0.172899083515371,0.00606748566075909,
1.00865535159306));
#20388=CARTESIAN_POINT('Ctrl Pts',(-0.0988016073770141,-0.142018132090297,
1.01659751971584));
#20389=CARTESIAN_POINT('Ctrl Pts',(0.0658082913934689,-0.160000550769587,
1.02453968783862));
#20390=CARTESIAN_POINT('Ctrl Pts',(0.170131034504888,-0.0314060274628177,
1.0324818559614));
#20391=CARTESIAN_POINT('Ctrl Pts',(0.118596271784576,0.125959643463681,
1.04042402408418));
#20392=CARTESIAN_POINT('Ctrl Pts',(-0.0415848597483297,0.167933340651612,
1.04836619220696));
#20393=CARTESIAN_POINT('Ctrl Pts',(-0.163669987576804,0.0560628453550813,
1.05630836032974));
#20394=CARTESIAN_POINT('Ctrl Pts',(-0.135816592328243,-0.107166975841641,
1.06425052845252));
#20395=CARTESIAN_POINT('Ctrl Pts',(0.0164587544616562,-0.172220837485682,
1.0721926965753));
#20396=CARTESIAN_POINT('Ctrl Pts',(0.153656191292587,-0.0795027190739688,
1.08013486469808));
#20397=CARTESIAN_POINT('Ctrl Pts',(0.150088771199207,0.0860480576341552,
1.08807703282086));
#20398=CARTESIAN_POINT('Ctrl Pts',(0.00902461748204118,0.172769973496559,
1.09601920094364));
#20399=CARTESIAN_POINT('Ctrl Pts',(-0.140307012982855,0.101216844302358,
1.10396136906642));
#20400=CARTESIAN_POINT('Ctrl Pts',(-0.161103005268346,-0.0630613126743013,
1.1119035371892));
#20401=CARTESIAN_POINT('Ctrl Pts',(-0.0343120939874615,-0.1695688287065,
1.11984570531198));
#20402=CARTESIAN_POINT('Ctrl Pts',(0.123912220401285,-0.120733877175888,
1.12778787343476));
#20403=CARTESIAN_POINT('Ctrl Pts',(0.168620210916381,0.0387057093103061,
1.13573004155754));
#20404=CARTESIAN_POINT('Ctrl Pts',(0.0588547652196237,0.162686889679659,
1.14367220968032));
#20405=CARTESIAN_POINT('Ctrl Pts',(-0.104827691798069,0.137630165643247,
1.1516143778031));
#20406=CARTESIAN_POINT('Ctrl Pts',(-0.172477213770776,-0.0135099294065116,
1.15955654592588));
#20407=CARTESIAN_POINT('Ctrl Pts',(-0.0821198886720452,-0.152273541192125,
1.16749871404866));
#20408=CARTESIAN_POINT('Ctrl Pts',(0.083467690946984,-0.15153894559049,
1.17544088217144));
#20409=CARTESIAN_POINT('Ctrl Pts',(0.172590290696882,-0.0119791076405788,
1.18338305029422));
#20410=CARTESIAN_POINT('Ctrl Pts',(0.103602453294194,0.13855482356859,1.191325218417));
#20411=CARTESIAN_POINT('Ctrl Pts',(-0.0602958748103966,0.162158302111078,
1.19926738653978));
#20412=CARTESIAN_POINT('Ctrl Pts',(-0.168956987158091,0.0372081167644847,
1.20720955466256));
#20413=CARTESIAN_POINT('Ctrl Pts',(-0.122836141658186,-0.121828526073448,
1.21515172278534));
#20414=CARTESIAN_POINT('Ctrl Pts',(0.0358152290369173,-0.169257723108079,
1.22309389090812));
#20415=CARTESIAN_POINT('Ctrl Pts',(0.161656170495932,-0.0616294572691503,
1.2310360590309));
#20416=CARTESIAN_POINT('Ctrl Pts',(0.13940345221127,0.102457722863032,1.23897822715368));
#20417=CARTESIAN_POINT('Ctrl Pts',(-0.0105571497596809,0.172683102970871,
1.24692039527646));
#20418=CARTESIAN_POINT('Ctrl Pts',(-0.150846317973597,0.0847130203482025,
1.25486256339924));
#20419=CARTESIAN_POINT('Ctrl Pts',(-0.152944761892581,-0.0808628918127005,
1.26280473152202));
#20420=CARTESIAN_POINT('Ctrl Pts',(-0.0149300913057054,-0.172360087712588,
1.2707468996448));
#20421=CARTESIAN_POINT('Ctrl Pts',(0.136762076743997,-0.105957736043287,
1.27868906776758));
#20422=CARTESIAN_POINT('Ctrl Pts',(0.163166132393764,0.0575127872937276,
1.28663123589036));
#20423=CARTESIAN_POINT('Ctrl Pts',(0.0400932480780463,0.168295688956082,
1.29457340401314));
#20424=CARTESIAN_POINT('Ctrl Pts',(-0.119709170414695,0.124902449862528,
1.30251557213592));
#20425=CARTESIAN_POINT('Ctrl Pts',(-0.169845690614082,-0.0329142650230248,
1.3104577402587));
#20426=CARTESIAN_POINT('Ctrl Pts',(-0.0643861093061943,-0.160578131733314,
1.31839990838148));
#20427=CARTESIAN_POINT('Ctrl Pts',(0.100057762773863,-0.141135932963798,
1.32634207650426));
#20428=CARTESIAN_POINT('Ctrl Pts',(0.172838444806952,0.00760127985757451,
1.33428424462704));
#20429=CARTESIAN_POINT('Ctrl Pts',(0.0872813550697656,0.149374939398002,
1.34222641274982));
#20430=CARTESIAN_POINT('Ctrl Pts',(-0.0782344227434143,0.154305808621531,
1.3501685808726));
#20431=CARTESIAN_POINT('Ctrl Pts',(-0.172079431848303,0.0178767046294837,
1.35811074899538));
#20432=CARTESIAN_POINT('Ctrl Pts',(-0.108282003268856,-0.134929297194493,
1.36605291711816));
#20433=CARTESIAN_POINT('Ctrl Pts',(0.0547128650701426,-0.164126201264144,
1.37399508524094));
#20434=CARTESIAN_POINT('Ctrl Pts',(0.167585127127835,-0.0429666431014547,
1.38193725336372));
#20435=CARTESIAN_POINT('Ctrl Pts',(0.126932197981417,0.117554773230619,
1.3898794214865));
#20436=CARTESIAN_POINT('Ctrl Pts',(-0.0300036684000219,0.170383942402052,
1.39782158960928));
#20437=CARTESIAN_POINT('Ctrl Pts',(-0.159453085214751,0.0671239123677834,
1.40576375773206));
#20438=CARTESIAN_POINT('Ctrl Pts',(-0.142827107870127,-0.0976285101620078,
1.41370592585484));
#20439=CARTESIAN_POINT('Ctrl Pts',(0.00464319840846943,-0.172943201171859,
1.42164809397762));
#20440=CARTESIAN_POINT('Ctrl Pts',(0.147859810582222,-0.0898241270588577,
1.4295902621004));
#20441=CARTESIAN_POINT('Ctrl Pts',(0.155621735944117,0.0755830265922534,
1.43753243022318));
#20442=CARTESIAN_POINT('Ctrl Pts',(0.0208179928734729,0.171748455656582,
1.44547459834596));
#20443=CARTESIAN_POINT('Ctrl Pts',(-0.133056846329205,0.11057447892796,
1.45341676646874));
#20444=CARTESIAN_POINT('Ctrl Pts',(-0.165038560097216,-0.0518967460486161,
1.46135893459152));
#20445=CARTESIAN_POINT('Ctrl Pts',(-0.0458268296361176,-0.166825854601292,
1.4693011027143));
#20446=CARTESIAN_POINT('Ctrl Pts',(0.115364766925686,-0.128924136976022,
1.47724327083708));
#20447=CARTESIAN_POINT('Ctrl Pts',(0.170874595884426,0.0270830477535184,
1.48518543895986));
#20448=CARTESIAN_POINT('Ctrl Pts',(0.0698377457337486,0.158283721017069,
1.49312760708264));
#20449=CARTESIAN_POINT('Ctrl Pts',(-0.0951624750893037,0.144471999488883,
1.50106977520542));
#20450=CARTESIAN_POINT('Ctrl Pts',(-0.173012914651864,-0.00167525885548286,
1.5090119433282));
#20451=CARTESIAN_POINT('Ctrl Pts',(-0.092311001583214,-0.14631755460685,
1.51695411145098));
#20452=CARTESIAN_POINT('Ctrl Pts',(0.072853104778531,-0.156861289272697,
1.52489627957376));
#20453=CARTESIAN_POINT('Ctrl Pts',(0.171475934783304,-0.0238129810547936,
1.53283844769654));
#20454=CARTESIAN_POINT('Ctrl Pts',(0.11261423476106,0.131269690464983,1.54078061581932));
#20455=CARTESIAN_POINT('Ctrl Pts',(0.00518264413773371,0.154149172621267,
1.54607539456784));
#20456=CARTESIAN_POINT('Ctrl Pts',(-0.0415060733757155,0.140340900570467,
1.5487227839421));
#20457=CARTESIAN_POINT('Ctrl Pts',(-0.146248097568756,-0.000123763188177425,
1.45893449541571));
#20458=CARTESIAN_POINT('Ctrl Pts',(-0.146367493381718,-0.0150081347743067,
1.45974264180765));
#20459=CARTESIAN_POINT('Ctrl Pts',(-0.144277648885518,-0.0298597803798721,
1.46055078819958));
#20460=CARTESIAN_POINT('Ctrl Pts',(-0.139839652725699,-0.043973059977961,
1.46135893459152));
#20461=CARTESIAN_POINT('Ctrl Pts',(-0.125301316610186,-0.0902064488995044,
1.46400632396578));
#20462=CARTESIAN_POINT('Ctrl Pts',(-0.08556407312315,-0.1285161517504,1.46665371334004));
#20463=CARTESIAN_POINT('Ctrl Pts',(-0.0388301852859989,-0.141354050238301,
1.4693011027143));
#20464=CARTESIAN_POINT('Ctrl Pts',(0.00790370255115092,-0.154191948726202,
1.47194849208856));
#20465=CARTESIAN_POINT('Ctrl Pts',(0.0616342347384179,-0.141558042851112,
1.47459588146282));
#20466=CARTESIAN_POINT('Ctrl Pts',(0.0977511389918415,-0.109239892458645,
1.47724327083708));
#20467=CARTESIAN_POINT('Ctrl Pts',(0.133868043245265,-0.0769217420661769,
1.47989066021134));
#20468=CARTESIAN_POINT('Ctrl Pts',(0.152371319564846,-0.024919347156331,
1.4825380495856));
#20469=CARTESIAN_POINT('Ctrl Pts',(0.144783482699524,0.0229486291758506,
1.48518543895986));
#20470=CARTESIAN_POINT('Ctrl Pts',(0.137195645834202,0.0708166055080336,
1.48783282833412));
#20471=CARTESIAN_POINT('Ctrl Pts',(0.103516695783975,0.114550163262552,
1.49048021770838));
#20472=CARTESIAN_POINT('Ctrl Pts',(0.0591771839550196,0.13411498855178,
1.49312760708264));
#20473=CARTESIAN_POINT('Ctrl Pts',(0.014837672126065,0.153679813841007,
1.4957749964569));
#20474=CARTESIAN_POINT('Ctrl Pts',(-0.0401624014816186,0.149075906664945,
1.49842238583116));
#20475=CARTESIAN_POINT('Ctrl Pts',(-0.0806375115458872,0.122416076686187,
1.50106977520542));
#20476=CARTESIAN_POINT('Ctrl Pts',(-0.0937869288003098,0.113754921033589,
1.50192985013695));
#20477=CARTESIAN_POINT('Ctrl Pts',(-0.105403311347291,0.102765876910903,
1.50278992506847));
#20478=CARTESIAN_POINT('Ctrl Pts',(-0.115078604842433,0.0902138214954038,
1.50365));
#20479=CARTESIAN_POINT('Ctrl Pts',(-0.0686146973663081,-0.0959584553529135,
1.07336015076065E-17));
#20480=CARTESIAN_POINT('Ctrl Pts',(-0.0712979561985307,-0.0944995001033786,
9.02613639135873E-18));
#20481=CARTESIAN_POINT('Ctrl Pts',(-0.0739152333025289,-0.0929325179580126,
1.64107321374712E-17));
#20482=CARTESIAN_POINT('Ctrl Pts',(-0.0764591723283171,-0.0912589988675934,
1.6154612370034E-17));
#20483=CARTESIAN_POINT('Ctrl Pts',(-0.0824897891353913,-0.0872917841461184,
1.52077426268717E-17));
#20484=CARTESIAN_POINT('Ctrl Pts',(-0.0881090519769445,-0.0827275518978924,
1.30971627060498E-17));
#20485=CARTESIAN_POINT('Ctrl Pts',(-0.0932912133381108,-0.0776621329443405,
1.43114686768087E-17));
#20486=CARTESIAN_POINT('Ctrl Pts',(-0.0960634919631888,-0.074952307504085,
1.49610807310118E-17));
#20487=CARTESIAN_POINT('Ctrl Pts',(-0.0987043519497191,-0.0721043812799658,
1.74993329480528E-17));
#20488=CARTESIAN_POINT('Ctrl Pts',(-0.101206237074718,-0.0691378820326018,
9.97465998686664E-18));
#20489=CARTESIAN_POINT('Ctrl Pts',(-0.105823426721714,-0.0636632543305198,
-3.91200561030858E-18));
#20490=CARTESIAN_POINT('Ctrl Pts',(-0.109972666997065,-0.0577811896139199,
2.24798207762934E-18));
#20491=CARTESIAN_POINT('Ctrl Pts',(-0.113625452403263,-0.0515741981665521,
9.54097911787244E-18));
#20492=CARTESIAN_POINT('Ctrl Pts',(-0.115386295340069,-0.0485820878086944,
1.30566037435822E-17));
#20493=CARTESIAN_POINT('Ctrl Pts',(-0.117027309103105,-0.0455212415157476,
-2.79521757168051E-18));
#20494=CARTESIAN_POINT('Ctrl Pts',(-0.118543833519887,-0.0424058589801268,
-3.46944695195361E-18));
#20495=CARTESIAN_POINT('Ctrl Pts',(-0.122700941917732,-0.0338659484069709,
-5.31764971597768E-18));
#20496=CARTESIAN_POINT('Ctrl Pts',(-0.125931492798984,-0.0249085743588085,
-1.15219401683824E-18));
#20497=CARTESIAN_POINT('Ctrl Pts',(-0.128167520083254,-0.0157105262534848,
9.54097911787244E-18));
#20498=CARTESIAN_POINT('Ctrl Pts',(-0.128992166906242,-0.0123182862745252,
1.3484621181291E-17));
#20499=CARTESIAN_POINT('Ctrl Pts',(-0.129681150280034,-0.00889298553317688,
1.10989611676181E-17));
#20500=CARTESIAN_POINT('Ctrl Pts',(-0.130229483957028,-0.00544263935519351,
9.54097911787244E-18));
#20501=CARTESIAN_POINT('Ctrl Pts',(-0.130761899349706,-0.00209245771889707,
8.02822573502553E-18));
#20502=CARTESIAN_POINT('Ctrl Pts',(-0.131160261982709,0.00127366115726457,
1.11791151702242E-17));
#20503=CARTESIAN_POINT('Ctrl Pts',(-0.131420990891747,0.00464012593483382,
8.67361737988404E-18));
#20504=CARTESIAN_POINT('Ctrl Pts',(-0.131728666658755,0.00861275649723166,
5.71697955546795E-18));
#20505=CARTESIAN_POINT('Ctrl Pts',(-0.131845259942619,0.0125891451047215,
-9.26473565962443E-18));
#20506=CARTESIAN_POINT('Ctrl Pts',(-0.131765781147177,0.0165567997877194,
-1.04083408558608E-17));
#20507=CARTESIAN_POINT('Ctrl Pts',(-0.131635692412819,0.0230509492424239,
-1.21888544026837E-17));
#20508=CARTESIAN_POINT('Ctrl Pts',(-0.13098103789945,0.0295216962360144,
-2.67049856555875E-17));
#20509=CARTESIAN_POINT('Ctrl Pts',(-0.129839098367345,0.0359278479980343,
-3.46944695195361E-17));
#20510=CARTESIAN_POINT('Ctrl Pts',(-0.129254890951344,0.0392051855997028,
-3.87818275556788E-17));
#20511=CARTESIAN_POINT('Ctrl Pts',(-0.128542951403208,0.0424656461998481,
-3.10678831811161E-17));
#20512=CARTESIAN_POINT('Ctrl Pts',(-0.1277070993652,0.0457037274559979,
-3.29597460435593E-17));
#20513=CARTESIAN_POINT('Ctrl Pts',(-0.126886363095037,0.0488832504000222,
-3.48173959609792E-17));
#20514=CARTESIAN_POINT('Ctrl Pts',(-0.125948031872817,0.0520333657183593,
-3.53366201082739E-17));
#20515=CARTESIAN_POINT('Ctrl Pts',(-0.124899042599898,0.0551436241923499,
-3.46944695195361E-17));
#20516=CARTESIAN_POINT('Ctrl Pts',(-0.122234979928128,0.0630425834229368,
-3.30636335736642E-17));
#20517=CARTESIAN_POINT('Ctrl Pts',(-0.118856305871375,0.070695441500891,
-2.1366080483524E-17));
#20518=CARTESIAN_POINT('Ctrl Pts',(-0.114834854776346,0.078019637496205,
-1.73472347597681E-17));
#20519=CARTESIAN_POINT('Ctrl Pts',(-0.11215901866562,0.0828930893082948,
-1.46731322388254E-17));
#20520=CARTESIAN_POINT('Ctrl Pts',(-0.109198005187061,0.0876211033078822,
8.28606628989234E-18));
#20521=CARTESIAN_POINT('Ctrl Pts',(-0.105966883726074,0.0921780034666525,
8.67361737988404E-18));
#20522=CARTESIAN_POINT('Ctrl Pts',(-0.104137243112614,0.094758373688769,
8.89307035390601E-18));
#20523=CARTESIAN_POINT('Ctrl Pts',(-0.102221042121924,0.0972831505018574,
-2.31209379389524E-17));
#20524=CARTESIAN_POINT('Ctrl Pts',(-0.100229777791505,0.0997373632832089,
-2.08166817117217E-17));
#20525=CARTESIAN_POINT('Ctrl Pts',(-0.0937202782075859,0.107760254486057,
-1.32840027382311E-17));
#20526=CARTESIAN_POINT('Ctrl Pts',(-0.0863914655699752,0.115060936709644,
5.4842312373535E-18));
#20527=CARTESIAN_POINT('Ctrl Pts',(-0.0783508402622743,0.121487309774744,
1.38777878078145E-17));
#20528=CARTESIAN_POINT('Ctrl Pts',(-0.073610711791116,0.125275800441382,
1.8825977152717E-17));
#20529=CARTESIAN_POINT('Ctrl Pts',(-0.068622257850438,0.128760167547443,
-9.09579695168528E-18));
#20530=CARTESIAN_POINT('Ctrl Pts',(-0.0634007094575209,0.131904027763685,
-6.93889390390723E-18));
#20531=CARTESIAN_POINT('Origin',(0.,0.,0.));
#20532=CARTESIAN_POINT('Origin',(-0.0721687836487033,-0.125,-0.3));
#20533=CARTESIAN_POINT('',(-0.0721687836487033,-0.125,-0.3));
#20534=CARTESIAN_POINT('',(0.0721687836487032,-0.125,-0.3));
#20535=CARTESIAN_POINT('',(-0.0360843918243517,-0.125,-0.3));
#20536=CARTESIAN_POINT('',(-0.0721687836487033,-0.125,-0.15));
#20537=CARTESIAN_POINT('',(-0.0721687836487033,-0.125,-0.3));
#20538=CARTESIAN_POINT('',(0.0721687836487032,-0.125,-0.15));
#20539=CARTESIAN_POINT('',(-0.0721687836487033,-0.125,-0.15));
#20540=CARTESIAN_POINT('',(0.0721687836487032,-0.125,-0.3));
#20541=CARTESIAN_POINT('Origin',(-0.144337567297406,1.76762539787485E-17,
-0.3));
#20542=CARTESIAN_POINT('',(-0.144337567297406,1.76762539787485E-17,-0.3));
#20543=CARTESIAN_POINT('',(-0.126295371385231,-0.03125,-0.3));
#20544=CARTESIAN_POINT('',(-0.144337567297406,2.77555756156289E-17,-0.15));
#20545=CARTESIAN_POINT('',(-0.144337567297406,1.76762539787485E-17,-0.3));
#20546=CARTESIAN_POINT('',(-0.144337567297406,1.76762539787485E-17,-0.15));
#20547=CARTESIAN_POINT('Origin',(-0.0721687836487032,0.125,-0.3));
#20548=CARTESIAN_POINT('',(-0.0721687836487032,0.125,-0.3));
#20549=CARTESIAN_POINT('',(-0.090210979560879,0.09375,-0.3));
#20550=CARTESIAN_POINT('',(-0.0721687836487032,0.125,-0.15));
#20551=CARTESIAN_POINT('',(-0.0721687836487032,0.125,-0.3));
#20552=CARTESIAN_POINT('',(-0.0721687836487032,0.125,-0.15));
#20553=CARTESIAN_POINT('Origin',(0.0721687836487032,0.125,-0.3));
#20554=CARTESIAN_POINT('',(0.0721687836487032,0.125,-0.3));
#20555=CARTESIAN_POINT('',(0.0360843918243516,0.125,-0.3));
#20556=CARTESIAN_POINT('',(0.0721687836487032,0.125,-0.15));
#20557=CARTESIAN_POINT('',(0.0721687836487032,0.125,-0.3));
#20558=CARTESIAN_POINT('',(0.0721687836487032,0.125,-0.15));
#20559=CARTESIAN_POINT('Origin',(0.144337567297406,0.,-0.3));
#20560=CARTESIAN_POINT('',(0.144337567297406,0.,-0.3));
#20561=CARTESIAN_POINT('',(0.126295371385231,0.03125,-0.3));
#20562=CARTESIAN_POINT('',(0.144337567297406,0.,-0.15));
#20563=CARTESIAN_POINT('',(0.144337567297406,0.,-0.3));
#20564=CARTESIAN_POINT('',(0.144337567297406,0.,-0.15));
#20565=CARTESIAN_POINT('Origin',(0.0721687836487032,-0.125,-0.3));
#20566=CARTESIAN_POINT('',(0.0902109795608791,-0.09375,-0.3));
#20567=CARTESIAN_POINT('',(0.0721687836487032,-0.125,-0.15));
#20568=CARTESIAN_POINT('Origin',(0.,0.,-0.15));
#20569=CARTESIAN_POINT('Origin',(0.,0.,0.));
#20570=CARTESIAN_POINT('',(-0.275,-3.36777869765522E-17,0.));
#20571=CARTESIAN_POINT('Origin',(0.,0.,0.));
#20572=CARTESIAN_POINT('Origin',(0.,0.,-0.3));
#20573=CARTESIAN_POINT('',(-0.275,-3.36777869765522E-17,-0.3));
#20574=CARTESIAN_POINT('',(-0.275,-3.36777869765522E-17,-0.3));
#20575=CARTESIAN_POINT('Origin',(0.,0.,-0.3));
#20576=CARTESIAN_POINT('Origin',(0.,0.,-0.3));
#20577=CARTESIAN_POINT('Origin',(0.,0.,1.6));
#20578=CARTESIAN_POINT('',(0.,0.,0.));
#20579=CARTESIAN_POINT('Origin',(0.,0.,0.12));
#20580=CARTESIAN_POINT('',(-0.12639138516214,8.91322620741042E-5,0.00934196736194174));
#20581=CARTESIAN_POINT('',(-0.12645,1.54856587752183E-17,-5.55111512312578E-17));
#20582=CARTESIAN_POINT('',(-0.12645,1.54856587752183E-17,0.12));
#20583=CARTESIAN_POINT('',(-0.0488748409397564,0.116622692573588,0.));
#20584=CARTESIAN_POINT('Origin',(0.,0.,0.));
#20585=CARTESIAN_POINT('Ctrl Pts',(-0.0489111879062984,0.116810626195002,
1.20007714660797E-17));
#20586=CARTESIAN_POINT('Ctrl Pts',(-0.0838963038512042,0.101957324585112,
0.00240024091002088));
#20587=CARTESIAN_POINT('Ctrl Pts',(-0.11198221847721,0.0702793053867637,
0.00480048182004174));
#20588=CARTESIAN_POINT('Ctrl Pts',(-0.122072221370749,0.0336561163696377,
0.00720072273006261));
#20589=CARTESIAN_POINT('Ctrl Pts',(-0.125072637487486,0.022765653033531,
0.00791447094068899));
#20590=CARTESIAN_POINT('Ctrl Pts',(-0.126481745582665,0.0114379076904012,
0.00862821915131536));
#20591=CARTESIAN_POINT('Ctrl Pts',(-0.12639138516214,8.91322620741042E-5,
0.00934196736194174));
#20592=CARTESIAN_POINT('Origin',(0.,0.,0.12));
#20593=CARTESIAN_POINT('',(-0.126396145829628,-9.95859796292312E-5,0.0593419673619417));
#20594=CARTESIAN_POINT('',(-0.126575671592806,-7.20628672610732E-5,0.0456580326380584));
#20595=CARTESIAN_POINT('',(-0.12645,1.54856587752183E-17,0.12));
#20596=CARTESIAN_POINT('',(-0.10808967569503,-0.0656218295092665,0.));
#20597=CARTESIAN_POINT('Ctrl Pts',(-0.126575671592806,-7.20628672610732E-5,
0.0456580326380584));
#20598=CARTESIAN_POINT('Ctrl Pts',(-0.126327459688109,0.0361497101693465,
0.0433719816070355));
#20599=CARTESIAN_POINT('Ctrl Pts',(-0.109912066394173,0.0725710138228805,
0.0410859305760125));
#20600=CARTESIAN_POINT('Ctrl Pts',(-0.0824515099939393,0.0961223418729112,
0.0387998795449896));
#20601=CARTESIAN_POINT('Ctrl Pts',(-0.05137998778939,0.122770586059505,
0.036213220908657));
#20602=CARTESIAN_POINT('Ctrl Pts',(-0.00616751748104999,0.132941603485868,
0.0336265622723243));
#20603=CARTESIAN_POINT('Ctrl Pts',(0.0333172074018229,0.122176268745047,
0.0310399036359917));
#20604=CARTESIAN_POINT('Ctrl Pts',(0.0728019322846963,0.111410934004226,
0.028453244999659));
#20605=CARTESIAN_POINT('Ctrl Pts',(0.106558911742102,0.0797092470962188,
0.0258665863633264));
#20606=CARTESIAN_POINT('Ctrl Pts',(0.11981357554495,0.0409763259700822,
0.0232799277269937));
#20607=CARTESIAN_POINT('Ctrl Pts',(0.133068239347797,0.00224340484394604,
0.0206932690906611));
#20608=CARTESIAN_POINT('Ctrl Pts',(0.125820587496086,-0.0435207505003201,
0.0181066104543285));
#20609=CARTESIAN_POINT('Ctrl Pts',(0.101166903546451,-0.0762076816581678,
0.0155199518179958));
#20610=CARTESIAN_POINT('Ctrl Pts',(0.0765132195968157,-0.108894612816016,
0.0129332931816632));
#20611=CARTESIAN_POINT('Ctrl Pts',(0.0344535035492562,-0.128504319787445,
0.0103466345453306));
#20612=CARTESIAN_POINT('Ctrl Pts',(-0.00636464094143544,-0.126469737202777,
0.00775997590899791));
#20613=CARTESIAN_POINT('Ctrl Pts',(-0.0471827854321269,-0.124435154618108,
0.00517331727266527));
#20614=CARTESIAN_POINT('Ctrl Pts',(-0.0867593583659505,-0.100756282477341,
0.00258665863633259));
#20615=CARTESIAN_POINT('Ctrl Pts',(-0.108089675695031,-0.0656218295092657,
-5.55111512312578E-17));
#20616=CARTESIAN_POINT('Origin',(0.,0.,0.));
#20617=CARTESIAN_POINT('Ctrl Pts',(-0.12639138516214,8.91322620741042E-5,
0.00934196736194174));
#20618=CARTESIAN_POINT('Ctrl Pts',(-0.126154274972366,-0.0296906128949183,
0.011214877787648));
#20619=CARTESIAN_POINT('Ctrl Pts',(-0.115592373032178,-0.0596151635265703,
0.0130877882133543));
#20620=CARTESIAN_POINT('Ctrl Pts',(-0.0963650578556872,-0.0821635787359664,
0.0149606986390606));
#20621=CARTESIAN_POINT('Ctrl Pts',(-0.0698103971670931,-0.113304978845907,
0.0175473572753932));
#20622=CARTESIAN_POINT('Ctrl Pts',(-0.0267272342632827,-0.130377059081323,
0.0201340159117258));
#20623=CARTESIAN_POINT('Ctrl Pts',(0.0139574509341311,-0.125868770046104,
0.0227206745480584));
#20624=CARTESIAN_POINT('Ctrl Pts',(0.0546421361315456,-0.121360481010885,
0.0253073331843911));
#20625=CARTESIAN_POINT('Ctrl Pts',(0.0929283436225635,-0.0952718227050311,
0.0278939918207237));
#20626=CARTESIAN_POINT('Ctrl Pts',(0.112018291148455,-0.0590635258734944,
0.0304806504570564));
#20627=CARTESIAN_POINT('Ctrl Pts',(0.131108238674346,-0.0228552290419586,
0.033067309093389));
#20628=CARTESIAN_POINT('Ctrl Pts',(0.131001926235112,0.0234727063152593,
0.0356539677297216));
#20629=CARTESIAN_POINT('Ctrl Pts',(0.111741771403992,0.0595891814911641,
0.0382406263660542));
#20630=CARTESIAN_POINT('Ctrl Pts',(0.0924816165728724,0.0957056566670696,
0.0408272850023869));
#20631=CARTESIAN_POINT('Ctrl Pts',(0.0540676193498672,0.121610671661662,
0.0434139436387195));
#20632=CARTESIAN_POINT('Ctrl Pts',(0.0133639835211523,0.125930636937597,
0.0460006022750522));
#20633=CARTESIAN_POINT('Ctrl Pts',(-0.0273396523075625,0.130250602213533,
0.0485872609113848));
#20634=CARTESIAN_POINT('Ctrl Pts',(-0.0703329267419868,0.112985517770812,
0.0511739195477175));
#20635=CARTESIAN_POINT('Ctrl Pts',(-0.0967449447385466,0.0817152626609385,
0.0537605781840501));
#20636=CARTESIAN_POINT('Ctrl Pts',(-0.115741878896724,0.0592240248649833,
0.0556210412433473));
#20637=CARTESIAN_POINT('Ctrl Pts',(-0.126160906676814,0.0294875554882879,
0.0574815043026445));
#20638=CARTESIAN_POINT('Ctrl Pts',(-0.126396145829628,-9.95859796292312E-5,
0.0593419673619417));
#20639=CARTESIAN_POINT('Origin',(0.,0.,0.12));
#20640=CARTESIAN_POINT('',(-0.126529791093031,9.025049583615E-5,0.109341967361942));
#20641=CARTESIAN_POINT('',(-0.126349242904067,8.85860673823967E-5,0.0956580326380584));
#20642=CARTESIAN_POINT('',(-0.12645,1.54856587752183E-17,0.12));
#20643=CARTESIAN_POINT('Ctrl Pts',(-0.126349242904067,8.85860673823967E-5,
0.0956580326380584));
#20644=CARTESIAN_POINT('Ctrl Pts',(-0.126441591528965,0.0135570965972842,
0.0948119253946973));
#20645=CARTESIAN_POINT('Ctrl Pts',(-0.124448136217638,0.0269990101701626,
0.0939658181513361));
#20646=CARTESIAN_POINT('Ctrl Pts',(-0.120249444863787,0.0397126388809939,
0.093119710907975));
#20647=CARTESIAN_POINT('Ctrl Pts',(-0.107413505522824,0.0785798365820317,
0.0905330522716423));
#20648=CARTESIAN_POINT('Ctrl Pts',(-0.0739673525896496,0.110640458354997,
0.0879463936353097));
#20649=CARTESIAN_POINT('Ctrl Pts',(-0.0345920580258737,0.121821308595361,
0.085359734998977));
#20650=CARTESIAN_POINT('Ctrl Pts',(0.00478323653790218,0.133002158835724,
0.0827730763626444));
#20651=CARTESIAN_POINT('Ctrl Pts',(0.0500876727322792,0.123303237543486,
0.0801864177263117));
#20652=CARTESIAN_POINT('Ctrl Pts',(0.0814342209129887,0.0969820390626645,
0.077599759089979));
#20653=CARTESIAN_POINT('Ctrl Pts',(0.112780769093698,0.0706608405818426,
0.0750131004536464));
#20654=CARTESIAN_POINT('Ctrl Pts',(0.13016942926074,0.0277173649124373,
0.0724264418173139));
#20655=CARTESIAN_POINT('Ctrl Pts',(0.12596827751407,-0.0129984006283456,
0.0698397831809812));
#20656=CARTESIAN_POINT('Ctrl Pts',(0.121767125767399,-0.0537141661691284,
0.0672531245446486));
#20657=CARTESIAN_POINT('Ctrl Pts',(0.0959761621070158,-0.0922022215812886,
0.0646664659083159));
#20658=CARTESIAN_POINT('Ctrl Pts',(0.059914723710966,-0.111567668284471,
0.0620798072719833));
#20659=CARTESIAN_POINT('Ctrl Pts',(0.0238532853149157,-0.130933114987654,
0.0594931486356506));
#20660=CARTESIAN_POINT('Ctrl Pts',(-0.0224786278168013,-0.131175952981858,
0.056906489999318));
#20661=CARTESIAN_POINT('Ctrl Pts',(-0.0587401909579078,-0.112190380850839,
0.0543198313629853));
#20662=CARTESIAN_POINT('Ctrl Pts',(-0.0950017540990138,-0.0932048087198191,
0.0517331727266527));
#20663=CARTESIAN_POINT('Ctrl Pts',(-0.12119296724951,-0.0549908264635757,
0.0491465140903201));
#20664=CARTESIAN_POINT('Ctrl Pts',(-0.125823286774378,-0.0143210998620416,
0.0465598554539874));
#20665=CARTESIAN_POINT('Ctrl Pts',(-0.126361397696569,-0.0095946821776348,
0.0462592478486778));
#20666=CARTESIAN_POINT('Ctrl Pts',(-0.12660831057823,-0.00483509759607578,
0.0459586402433681));
#20667=CARTESIAN_POINT('Ctrl Pts',(-0.126575671592806,-7.20628672610732E-5,
0.0456580326380584));
#20668=CARTESIAN_POINT('Ctrl Pts',(-0.126396145829628,-9.95859796292312E-5,
0.0593419673619417));
#20669=CARTESIAN_POINT('Ctrl Pts',(-0.12648796685852,-0.0116483513064931,
0.0600681629389771));
#20670=CARTESIAN_POINT('Ctrl Pts',(-0.125028206814926,-0.0231743653405588,
0.0607943585160125));
#20671=CARTESIAN_POINT('Ctrl Pts',(-0.121921363946098,-0.034237873926493,
0.0615205540930479));
#20672=CARTESIAN_POINT('Ctrl Pts',(-0.110855003598394,-0.0736453296270277,
0.0641072127293806));
#20673=CARTESIAN_POINT('Ctrl Pts',(-0.0788915213442898,-0.107184815251071,
0.0666938713657133));
#20674=CARTESIAN_POINT('Ctrl Pts',(-0.0400617348236378,-0.120133683626334,
0.069280530002046));
#20675=CARTESIAN_POINT('Ctrl Pts',(-0.00123194830298627,-0.133082552001597,
0.0718671886383786));
#20676=CARTESIAN_POINT('Ctrl Pts',(0.0444641424842127,-0.125440803128081,
0.0744538472747112));
#20677=CARTESIAN_POINT('Ctrl Pts',(0.0769682295152699,-0.100563001286921,
0.0770405059110438));
#20678=CARTESIAN_POINT('Ctrl Pts',(0.109472316546327,-0.0756851994457607,
0.0796271645473764));
#20679=CARTESIAN_POINT('Ctrl Pts',(0.128784399821243,-0.0335713446369571,
0.0822138231837091));
#20680=CARTESIAN_POINT('Ctrl Pts',(0.126427276285523,0.00729262199647547,
0.0848004818200417));
#20681=CARTESIAN_POINT('Ctrl Pts',(0.124070152749803,0.0481565886299079,
0.0873871404563744));
#20682=CARTESIAN_POINT('Ctrl Pts',(0.100043822403448,0.0877706670879697,
0.0899737990927071));
#20683=CARTESIAN_POINT('Ctrl Pts',(0.0648947831756147,0.108746049780439,
0.0925604577290397));
#20684=CARTESIAN_POINT('Ctrl Pts',(0.0297457439477817,0.129721432472907,
0.0951471163653723));
#20685=CARTESIAN_POINT('Ctrl Pts',(-0.0165260041615291,0.132058119399784,
0.0977337750017049));
#20686=CARTESIAN_POINT('Ctrl Pts',(-0.0536093211433369,0.114730442741844,
0.100320433638038));
#20687=CARTESIAN_POINT('Ctrl Pts',(-0.0906926381251451,0.0974027660839045,
0.10290709227437));
#20688=CARTESIAN_POINT('Ctrl Pts',(-0.11858752397945,0.0604107258411485,
0.105493750910703));
#20689=CARTESIAN_POINT('Ctrl Pts',(-0.12504939731921,0.0199921027543164,
0.108080409547035));
#20690=CARTESIAN_POINT('Ctrl Pts',(-0.126099919499473,0.0134211506765118,
0.108500928818671));
#20691=CARTESIAN_POINT('Ctrl Pts',(-0.126583971845017,0.00675963476331471,
0.108921448090306));
#20692=CARTESIAN_POINT('Ctrl Pts',(-0.126529791093031,9.025049583615E-5,
0.109341967361942));
#20693=CARTESIAN_POINT('Origin',(0.,0.,0.12));
#20694=CARTESIAN_POINT('',(-0.126296536029262,-6.10717992316628E-5,0.159341967361942));
#20695=CARTESIAN_POINT('',(-0.126453631260982,-0.000102348163238207,0.145658032638058));
#20696=CARTESIAN_POINT('',(-0.12645,1.54856587752183E-17,0.12));
#20697=CARTESIAN_POINT('Ctrl Pts',(-0.126453631260982,-0.000102348163238207,
0.145658032638058));
#20698=CARTESIAN_POINT('Ctrl Pts',(-0.126183364177612,0.031552920325249,
0.143665210546026));
#20699=CARTESIAN_POINT('Ctrl Pts',(-0.114073771100105,0.0633928690595716,
0.141672388453994));
#20700=CARTESIAN_POINT('Ctrl Pts',(-0.0925489356314354,0.0864391430514358,
0.139679566361962));
#20701=CARTESIAN_POINT('Ctrl Pts',(-0.0646099631645552,0.116352924063146,
0.13709290772563));
#20702=CARTESIAN_POINT('Ctrl Pts',(-0.0208084524006029,0.131451366650306,
0.134506249089297));
#20703=CARTESIAN_POINT('Ctrl Pts',(0.0196287675426836,0.125106932552633,
0.131919590452964));
#20704=CARTESIAN_POINT('Ctrl Pts',(0.0600659874859703,0.11876249845496,
0.129332931816632));
#20705=CARTESIAN_POINT('Ctrl Pts',(0.097138916608591,0.0909751876724545,
0.126746273180299));
#20706=CARTESIAN_POINT('Ctrl Pts',(0.114574233156503,0.0539423598350403,
0.124159614543967));
#20707=CARTESIAN_POINT('Ctrl Pts',(0.132009549704415,0.0169095319976262,
0.121572955907634));
#20708=CARTESIAN_POINT('Ctrl Pts',(0.129807253677619,-0.0293688128946969,
0.118986297271301));
#20709=CARTESIAN_POINT('Ctrl Pts',(0.108934072954415,-0.0645786240759305,
0.116399638634969));
#20710=CARTESIAN_POINT('Ctrl Pts',(0.0880608922312115,-0.099788435257164,
0.113812979998636));
#20711=CARTESIAN_POINT('Ctrl Pts',(0.0485168268116012,-0.123929712727308,
0.111226321362303));
#20712=CARTESIAN_POINT('Ctrl Pts',(0.00765986125275547,-0.126405537442516,
0.108639662725971));
#20713=CARTESIAN_POINT('Ctrl Pts',(-0.0331971043060904,-0.128881362157723,
0.106053004089638));
#20714=CARTESIAN_POINT('Ctrl Pts',(-0.0753669700041717,-0.109691734117994,
0.103466345453305));
#20715=CARTESIAN_POINT('Ctrl Pts',(-0.100339039978837,-0.0772600332835736,
0.100879686816973));
#20716=CARTESIAN_POINT('Ctrl Pts',(-0.117142637704978,-0.0554368822612891,
0.0991391354240014));
#20717=CARTESIAN_POINT('Ctrl Pts',(-0.126159269908366,-0.0276178718881664,
0.0973985840310299));
#20718=CARTESIAN_POINT('Ctrl Pts',(-0.126349242904067,8.85860673823967E-5,
0.0956580326380584));
#20719=CARTESIAN_POINT('Ctrl Pts',(-0.126529791093031,9.025049583615E-5,
0.109341967361942));
#20720=CARTESIAN_POINT('Ctrl Pts',(-0.126250700293628,-0.0342644551610371,
0.111508106726639));
#20721=CARTESIAN_POINT('Ctrl Pts',(-0.111690189779818,-0.0688279388928191,
0.113674246091336));
#20722=CARTESIAN_POINT('Ctrl Pts',(-0.0867076257192948,-0.092297473337895,
0.115840385456033));
#20723=CARTESIAN_POINT('Ctrl Pts',(-0.0568751199544048,-0.120323220412367,
0.118427044092366));
#20724=CARTESIAN_POINT('Ctrl Pts',(-0.0121812475994092,-0.132529508630403,
0.121013702728699));
#20725=CARTESIAN_POINT('Ctrl Pts',(0.0277554439013372,-0.123558363290506,
0.123600361365031));
#20726=CARTESIAN_POINT('Ctrl Pts',(0.0676921354020838,-0.114587217950609,
0.126187020001364));
#20727=CARTESIAN_POINT('Ctrl Pts',(0.102871646048582,-0.0844386390527785,
0.128773678637697));
#20728=CARTESIAN_POINT('Ctrl Pts',(0.117851793294146,-0.0463464242807743,
0.131360337274029));
#20729=CARTESIAN_POINT('Ctrl Pts',(0.13283194053971,-0.00825420950877041,
0.133946995910362));
#20730=CARTESIAN_POINT('Ctrl Pts',(0.127612724384341,0.0377816411374068,
0.136533654546694));
#20731=CARTESIAN_POINT('Ctrl Pts',(0.104485135941302,0.0715534408109559,
0.139120313183027));
#20732=CARTESIAN_POINT('Ctrl Pts',(0.0813575474982633,0.105325240484505,
0.14170697181936));
#20733=CARTESIAN_POINT('Ctrl Pts',(0.0403215867675544,0.126832989185426,
0.144293630455692));
#20734=CARTESIAN_POINT('Ctrl Pts',(-0.000609841963000384,0.126635909896556,
0.146880289092025));
#20735=CARTESIAN_POINT('Ctrl Pts',(-0.0415412706935549,0.126438830607686,
0.149466947728358));
#20736=CARTESIAN_POINT('Ctrl Pts',(-0.0823681674239554,0.104536923329025,
0.15205360636469));
#20737=CARTESIAN_POINT('Ctrl Pts',(-0.10516942503222,0.0705438627883669,
0.154640265001023));
#20738=CARTESIAN_POINT('Ctrl Pts',(-0.118984510025511,0.0499477610899654,
0.156207499121329));
#20739=CARTESIAN_POINT('Ctrl Pts',(-0.126182304652747,0.0249129445447297,
0.157774733241635));
#20740=CARTESIAN_POINT('Ctrl Pts',(-0.126296536029262,-6.10717992316628E-5,
0.159341967361942));
#20741=CARTESIAN_POINT('Origin',(0.,0.,0.12));
#20742=CARTESIAN_POINT('',(-0.126625441102054,2.7778768752873E-5,0.209341967361942));
#20743=CARTESIAN_POINT('',(-0.126471935391749,0.000101176582396995,0.195658032638058));
#20744=CARTESIAN_POINT('',(-0.12645,1.54856587752183E-17,0.12));
#20745=CARTESIAN_POINT('',(0.0958116152722397,0.0825211298936481,0.24));
#20746=CARTESIAN_POINT('Ctrl Pts',(-0.126625441102054,2.7778768752873E-5,
0.209341967361942));
#20747=CARTESIAN_POINT('Ctrl Pts',(-0.126482885932031,-0.0388928622545336,
0.21180133566563));
#20748=CARTESIAN_POINT('Ctrl Pts',(-0.107125339127294,-0.077921419747323,
0.214260703969318));
#20749=CARTESIAN_POINT('Ctrl Pts',(-0.0759952538809665,-0.101287130411732,
0.216720072273006));
#20750=CARTESIAN_POINT('Ctrl Pts',(-0.0432539585932993,-0.12586218783339,
0.219306730909339));
#20751=CARTESIAN_POINT('Ctrl Pts',(0.0025100419330305,-0.133111106253138,
0.221893389545672));
#20752=CARTESIAN_POINT('Ctrl Pts',(0.0412155518054008,-0.119764891216682,
0.224480048182004));
#20753=CARTESIAN_POINT('Ctrl Pts',(0.0799210616777711,-0.106418676180227,
0.227066706818337));
#20754=CARTESIAN_POINT('Ctrl Pts',(0.111568080896182,-0.072477327687567,
0.229653365454669));
#20755=CARTESIAN_POINT('Ctrl Pts',(0.122246574267713,-0.0330282462555153,
0.232240024091002));
#20756=CARTESIAN_POINT('Ctrl Pts',(0.132925067639245,0.00642083517653631,
0.234826682727335));
#20757=CARTESIAN_POINT('Ctrl Pts',(0.122635035163896,0.0513776495479799,
0.237413341363667));
#20758=CARTESIAN_POINT('Ctrl Pts',(0.0958116152722397,0.0825211298936481,
0.24));
#20759=CARTESIAN_POINT('',(-0.0959791030802601,0.0826138105732953,0.24));
#20760=CARTESIAN_POINT('Origin',(0.,0.,0.24));
#20761=CARTESIAN_POINT('Ctrl Pts',(-0.0959791030802601,0.0826138105732953,
0.24));
#20762=CARTESIAN_POINT('Ctrl Pts',(-0.0710417758635208,0.111296717646776,
0.237599759089979));
#20763=CARTESIAN_POINT('Ctrl Pts',(-0.0322351762885183,0.128218895525122,
0.235199518179958));
#20764=CARTESIAN_POINT('Ctrl Pts',(0.00571352152256588,0.126497857083363,
0.232799277269937));
#20765=CARTESIAN_POINT('Ctrl Pts',(0.0466095526337785,0.124643152028446,
0.230212618633605));
#20766=CARTESIAN_POINT('Ctrl Pts',(0.0865092470399708,0.101136876245298,
0.227625959997272));
#20767=CARTESIAN_POINT('Ctrl Pts',(0.107920636628548,0.0662586835305903,
0.225039301360939));
#20768=CARTESIAN_POINT('Ctrl Pts',(0.129332026217125,0.0313804908158828,
0.222452642724607));
#20769=CARTESIAN_POINT('Ctrl Pts',(0.132255110988087,-0.014869618830384,
0.219865984088274));
#20770=CARTESIAN_POINT('Ctrl Pts',(0.115395215428634,-0.0521699181865619,
0.217279325451942));
#20771=CARTESIAN_POINT('Ctrl Pts',(0.0985353198691812,-0.0894702175427398,
0.214692666815609));
#20772=CARTESIAN_POINT('Ctrl Pts',(0.0618924439793129,-0.117820706608829,
0.212106008179276));
#20773=CARTESIAN_POINT('Ctrl Pts',(0.0215571925812854,-0.12478734248304,
0.209519349542944));
#20774=CARTESIAN_POINT('Ctrl Pts',(-0.0187780588167422,-0.13175397835725,
0.206932690906611));
#20775=CARTESIAN_POINT('Ctrl Pts',(-0.0628056857229291,-0.117336761039583,
0.204346032270278));
#20776=CARTESIAN_POINT('Ctrl Pts',(-0.0912027768750998,-0.0878586653637446,
0.201759373633946));
#20777=CARTESIAN_POINT('Ctrl Pts',(-0.113530209130371,-0.0646812849521466,
0.199725593301983));
#20778=CARTESIAN_POINT('Ctrl Pts',(-0.126194825294183,-0.0321932513395888,
0.197691812970021));
#20779=CARTESIAN_POINT('Ctrl Pts',(-0.126471935391749,0.000101176582396995,
0.195658032638058));
#20780=CARTESIAN_POINT('Origin',(0.,0.,0.350421172358873));
#20781=CARTESIAN_POINT('',(-0.154453350152392,-8.79343647196378E-5,0.0295788276411275));
#20782=CARTESIAN_POINT('',(-0.15422847552802,0.000108763211052777,0.025421172358873));
#20783=CARTESIAN_POINT('',(-0.1543,-1.01731279388251E-15,0.350421172358873));
#20784=CARTESIAN_POINT('',(0.15408394018464,-0.00816268198427004,0.));
#20785=CARTESIAN_POINT('Ctrl Pts',(-0.15422847552802,0.000108763211052763,
0.025421172358873));
#20786=CARTESIAN_POINT('Ctrl Pts',(-0.154338737393477,0.0139570514561378,
0.0247074241482466));
#20787=CARTESIAN_POINT('Ctrl Pts',(-0.146387882101843,0.0778735560251454,
0.0214070173012875));
#20788=CARTESIAN_POINT('Ctrl Pts',(-0.0581466660421577,0.171532975008042,
0.0155199518179959));
#20789=CARTESIAN_POINT('Ctrl Pts',(0.109502662757235,0.144085240745689,
0.00775997590899784));
#20790=CARTESIAN_POINT('Ctrl Pts',(0.156737212705124,0.0419221657566679,
0.00258665863633264));
#20791=CARTESIAN_POINT('Ctrl Pts',(0.15408394018464,-0.00816268198427004,
0.));
#20792=CARTESIAN_POINT('',(0.129620323775263,-0.0841289546921688,3.62607491890453E-17));
#20793=CARTESIAN_POINT('Origin',(0.,0.,0.));
#20794=CARTESIAN_POINT('Ctrl Pts',(-0.154453350152392,-8.7934364719636E-5,
0.0295788276411275));
#20795=CARTESIAN_POINT('Ctrl Pts',(-0.154150470777978,0.0441115087317509,
0.0272927766101045));
#20796=CARTESIAN_POINT('Ctrl Pts',(-0.111454882743928,0.138841433785012,
0.0224200669427489));
#20797=CARTESIAN_POINT('Ctrl Pts',(0.0476444145610997,0.174632482457551,
0.0149606986390605));
#20798=CARTESIAN_POINT('Ctrl Pts',(0.168251138196633,0.0613688951001999,
0.0073871404563744));
#20799=CARTESIAN_POINT('Ctrl Pts',(0.154676764047789,-0.0451013867871701,
0.00240024091002087));
#20800=CARTESIAN_POINT('Ctrl Pts',(0.129620323775263,-0.0841289546921688,
1.57209315010398E-17));
#20801=CARTESIAN_POINT('Origin',(0.,0.,0.350421172358873));
#20802=CARTESIAN_POINT('',(-0.154177051641736,0.000108096719625833,0.0795788276411275));
#20803=CARTESIAN_POINT('',(-0.154234284709463,-0.000121519309271207,0.075421172358873));
#20804=CARTESIAN_POINT('',(-0.1543,-1.01731279388251E-15,0.350421172358873));
#20805=CARTESIAN_POINT('Ctrl Pts',(-0.154234284709463,-0.000121519309271208,
0.0754211723588731));
#20806=CARTESIAN_POINT('Ctrl Pts',(-0.153947235272697,0.0359820467524117,
0.0735607092995758));
#20807=CARTESIAN_POINT('Ctrl Pts',(-0.123557126730793,0.122717061869437,
0.0691135876039459));
#20808=CARTESIAN_POINT('Ctrl Pts',(0.0191012565771036,0.180005302104073,
0.0620798072719832));
#20809=CARTESIAN_POINT('Ctrl Pts',(0.159724738700703,0.0851738948996701,
0.0543198313629854));
#20810=CARTESIAN_POINT('Ctrl Pts',(0.160113920417758,-0.0844204212478698,
0.0465598554539874));
#20811=CARTESIAN_POINT('Ctrl Pts',(0.0199582426985643,-0.179924098035372,
0.0387998795449896));
#20812=CARTESIAN_POINT('Ctrl Pts',(-0.123251388539896,-0.123176028715441,
0.0317536518466181));
#20813=CARTESIAN_POINT('Ctrl Pts',(-0.153939142967466,-0.0362298265692857,
0.0272940827845792));
#20814=CARTESIAN_POINT('Ctrl Pts',(-0.15422847552802,0.000108763211052763,
0.025421172358873));
#20815=CARTESIAN_POINT('Ctrl Pts',(-0.154177051641736,0.000108096719625859,
0.0795788276411275));
#20816=CARTESIAN_POINT('Ctrl Pts',(-0.154289739603949,0.0165429814548096,
0.0787327203977663));
#20817=CARTESIAN_POINT('Ctrl Pts',(-0.144420757340354,0.0830897487115299,
0.0752999545180725));
#20818=CARTESIAN_POINT('Ctrl Pts',(-0.0494457976037486,0.174130301808973,
0.0692805300020459));
#20819=CARTESIAN_POINT('Ctrl Pts',(0.11640175885633,0.13862511662766,0.061520554093048));
#20820=CARTESIAN_POINT('Ctrl Pts',(0.18005704388064,-0.0185795878987759,
0.0537605781840501));
#20821=CARTESIAN_POINT('Ctrl Pts',(0.0856431484406112,-0.159474177462153,
0.0460006022750521));
#20822=CARTESIAN_POINT('Ctrl Pts',(-0.0839657292871194,-0.160363143120653,
0.0382406263660544));
#20823=CARTESIAN_POINT('Ctrl Pts',(-0.151599316432495,-0.0616831513139142,
0.0327667014880793));
#20824=CARTESIAN_POINT('Ctrl Pts',(-0.154493177716258,-0.00590000442131094,
0.0298794352464371));
#20825=CARTESIAN_POINT('Ctrl Pts',(-0.154453350152392,-8.7934364719636E-5,
0.0295788276411275));
#20826=CARTESIAN_POINT('Origin',(0.,0.,0.350421172358873));
#20827=CARTESIAN_POINT('',(-0.154304431028624,-0.000124889850439479,0.129578827641127));
#20828=CARTESIAN_POINT('',(-0.154397364694779,0.000110127730384366,0.125421172358873));
#20829=CARTESIAN_POINT('',(-0.1543,-1.01731279388251E-15,0.350421172358873));
#20830=CARTESIAN_POINT('Ctrl Pts',(-0.154397364694779,0.000110127730384357,
0.125421172358873));
#20831=CARTESIAN_POINT('Ctrl Pts',(-0.154463478494948,0.00824841157753406,
0.125000653087238));
#20832=CARTESIAN_POINT('Ctrl Pts',(-0.150239588102603,0.0663774823757793,
0.121993475179269));
#20833=CARTESIAN_POINT('Ctrl Pts',(-0.0766286530280003,0.163994611436961,
0.116399638634969));
#20834=CARTESIAN_POINT('Ctrl Pts',(0.0927599764682439,0.155440618724813,
0.108639662725971));
#20835=CARTESIAN_POINT('Ctrl Pts',(0.180714016146597,0.0104239566588842,
0.100879686816973));
#20836=CARTESIAN_POINT('Ctrl Pts',(0.11001758793024,-0.143743725357685,
0.093119710907975));
#20837=CARTESIAN_POINT('Ctrl Pts',(-0.0572637123892103,-0.171718146500831,
0.0853597349989769));
#20838=CARTESIAN_POINT('Ctrl Pts',(-0.146220320052713,-0.0783754111826042,
0.0794602221492764));
#20839=CARTESIAN_POINT('Ctrl Pts',(-0.154346328875204,-0.0142138442593302,
0.0761473679359084));
#20840=CARTESIAN_POINT('Ctrl Pts',(-0.154234284709463,-0.000121519309271208,
0.0754211723588731));
#20841=CARTESIAN_POINT('Ctrl Pts',(-0.154304431028624,-0.000124889850439474,
0.129578827641127));
#20842=CARTESIAN_POINT('Ctrl Pts',(-0.153974638929265,0.0385022981904757,
0.127586005549095));
#20843=CARTESIAN_POINT('Ctrl Pts',(-0.120018027207353,0.127784966030512,
0.123006524820731));
#20844=CARTESIAN_POINT('Ctrl Pts',(0.0280571680938306,0.178826694862324,
0.115840385456033));
#20845=CARTESIAN_POINT('Ctrl Pts',(0.163771354656592,0.0771047007047774,
0.108080409547035));
#20846=CARTESIAN_POINT('Ctrl Pts',(0.155709331479018,-0.0923080778690166,
0.100320433638038));
#20847=CARTESIAN_POINT('Ctrl Pts',(0.0109489686262093,-0.180682908560435,
0.0925604577290397));
#20848=CARTESIAN_POINT('Ctrl Pts',(-0.126591758993125,-0.118094248159534,
0.0856465890634029));
#20849=CARTESIAN_POINT('Ctrl Pts',(-0.153945238013925,-0.0337005743957639,
0.0813193790340989));
#20850=CARTESIAN_POINT('Ctrl Pts',(-0.154177051641736,0.000108096719625859,
0.0795788276411275));
#20851=CARTESIAN_POINT('Origin',(0.,0.,0.350421172358873));
#20852=CARTESIAN_POINT('',(-0.154326766555531,0.000123460234585843,0.179578827641127));
#20853=CARTESIAN_POINT('',(-0.154112736333057,-7.45225671948511E-5,0.175421172358873));
#20854=CARTESIAN_POINT('',(-0.1543,-1.01731279388251E-15,0.350421172358873));
#20855=CARTESIAN_POINT('Ctrl Pts',(-0.154112736333057,-7.45225671948471E-5,
0.175421172358873));
#20856=CARTESIAN_POINT('Ctrl Pts',(-0.153973346049181,0.0303998999070902,
0.173853938238567));
#20857=CARTESIAN_POINT('Ctrl Pts',(-0.130694151755309,0.111367805862998,
0.169700045481928));
#20858=CARTESIAN_POINT('Ctrl Pts',(-0.000871711368246156,0.181012066871201,
0.162959494088956));
#20859=CARTESIAN_POINT('Ctrl Pts',(0.149350085565286,0.102277888352765,
0.155199518179958));
#20860=CARTESIAN_POINT('Ctrl Pts',(0.168456255263351,-0.0662471829332422,
0.14743954227096));
#20861=CARTESIAN_POINT('Ctrl Pts',(0.0396733728729688,-0.17661315503135,
0.139679566361963));
#20862=CARTESIAN_POINT('Ctrl Pts',(-0.115072782317819,-0.134350623919955,
0.1323401097246));
#20863=CARTESIAN_POINT('Ctrl Pts',(-0.154056805498669,-0.041811035439686,
0.12758731172357));
#20864=CARTESIAN_POINT('Ctrl Pts',(-0.154397364694779,0.000110127730384357,
0.125421172358873));
#20865=CARTESIAN_POINT('Ctrl Pts',(-0.154326766555531,0.000123460234585825,
0.179578827641127));
#20866=CARTESIAN_POINT('Ctrl Pts',(-0.154418689716183,0.0108361910665024,
0.179025949336757));
#20867=CARTESIAN_POINT('Ctrl Pts',(-0.148597337680631,0.071569631208062,
0.175886412396054));
#20868=CARTESIAN_POINT('Ctrl Pts',(-0.0683530255288039,0.167611467503216,
0.170160216819019));
#20869=CARTESIAN_POINT('Ctrl Pts',(0.100397202365132,0.150621028353064,
0.162400240910021));
#20870=CARTESIAN_POINT('Ctrl Pts',(0.18100910679194,0.00139719974911195,
0.154640265001023));
#20871=CARTESIAN_POINT('Ctrl Pts',(0.102711092909207,-0.149052183789333,
0.146880289092025));
#20872=CARTESIAN_POINT('Ctrl Pts',(-0.0657574679958034,-0.168648048308422,
0.139120313183027));
#20873=CARTESIAN_POINT('Ctrl Pts',(-0.148058381688037,-0.0731761882111772,
0.133353159366061));
#20874=CARTESIAN_POINT('Ctrl Pts',(-0.154402705029802,-0.0116353181791797,
0.130172664185428));
#20875=CARTESIAN_POINT('Ctrl Pts',(-0.154304431028624,-0.000124889850439474,
0.129578827641127));
#20876=CARTESIAN_POINT('Origin',(0.,0.,0.350421172358873));
#20877=CARTESIAN_POINT('',(-0.154128406284035,-0.000157308197905263,0.229578827641128));
#20878=CARTESIAN_POINT('',(-0.154514081154978,3.38969080117728E-5,0.225421172358873));
#20879=CARTESIAN_POINT('',(-0.1543,-1.01731279388251E-15,0.350421172358873));
#20880=CARTESIAN_POINT('',(-0.0398513841857245,-0.149064942821851,0.24));
#20881=CARTESIAN_POINT('Ctrl Pts',(-0.0398513841857245,-0.149064942821851,
0.24));
#20882=CARTESIAN_POINT('Ctrl Pts',(-0.0883048112969314,-0.136111285829332,
0.237413341363667));
#20883=CARTESIAN_POINT('Ctrl Pts',(-0.143745772087175,-0.0847488633265083,
0.233939617244043));
#20884=CARTESIAN_POINT('Ctrl Pts',(-0.154234229255939,-0.017399338864059,
0.230465893124419));
#20885=CARTESIAN_POINT('Ctrl Pts',(-0.154128406284035,-0.00015730819790527,
0.229578827641128));
#20886=CARTESIAN_POINT('',(0.0399565498027962,-0.149273502906638,0.24));
#20887=CARTESIAN_POINT('Origin',(0.,0.,0.24));
#20888=CARTESIAN_POINT('Ctrl Pts',(0.0399565498027963,-0.149273502906638,
0.24));
#20889=CARTESIAN_POINT('Ctrl Pts',(-0.00490373130458673,-0.161043406468747,
0.237599759089979));
#20890=CARTESIAN_POINT('Ctrl Pts',(-0.107666111297752,-0.141562671532916,
0.23274014987627));
#20891=CARTESIAN_POINT('Ctrl Pts',(-0.154340128899266,-0.0474588267763927,
0.227880540662561));
#20892=CARTESIAN_POINT('Ctrl Pts',(-0.154514081154978,3.3896908011755E-5,
0.225421172358873));
#20893=CARTESIAN_POINT('Origin',(0.,0.,0.350421172358873));
#20894=CARTESIAN_POINT('Ctrl Pts',(-0.154514081154978,3.3896908011755E-5,
0.225421172358873));
#20895=CARTESIAN_POINT('Ctrl Pts',(-0.154523084458981,0.00249199339844659,
0.225293882026228));
#20896=CARTESIAN_POINT('Ctrl Pts',(-0.153375868586475,0.0548933889046004,
0.222579933057251));
#20897=CARTESIAN_POINT('Ctrl Pts',(-0.0942515706791253,0.154556313135293,
0.217279325451942));
#20898=CARTESIAN_POINT('Ctrl Pts',(0.0750450248431312,0.164716481511431,
0.209519349542944));
#20899=CARTESIAN_POINT('Ctrl Pts',(0.178461260043253,0.0303012077178856,
0.201759373633945));
#20900=CARTESIAN_POINT('Ctrl Pts',(0.125203781387627,-0.130731709675357,
0.193999397724948));
#20901=CARTESIAN_POINT('Ctrl Pts',(-0.0379704533096903,-0.17698585337688,
0.18623942181595));
#20902=CARTESIAN_POINT('Ctrl Pts',(-0.141587477595567,-0.0899051669249145,
0.180046680027258));
#20903=CARTESIAN_POINT('Ctrl Pts',(-0.154203404262525,-0.019896942829432,
0.176440596874899));
#20904=CARTESIAN_POINT('Ctrl Pts',(-0.154112736333057,-7.45225671948471E-5,
0.175421172358873));
#20905=CARTESIAN_POINT('Ctrl Pts',(-0.154128406284035,-0.00015730819790527,
0.229578827641128));
#20906=CARTESIAN_POINT('Ctrl Pts',(-0.153925652370292,0.0328779499839183,
0.227879234488086));
#20907=CARTESIAN_POINT('Ctrl Pts',(-0.127638532780061,0.116591914860373,
0.223592982698713));
#20908=CARTESIAN_POINT('Ctrl Pts',(0.00818767200092134,0.180778621679153,
0.216720072273006));
#20909=CARTESIAN_POINT('Ctrl Pts',(0.154249898498561,0.0947283641859207,
0.208960096364008));
#20910=CARTESIAN_POINT('Ctrl Pts',(0.164950538597243,-0.0745810526211722,
0.201200120455011));
#20911=CARTESIAN_POINT('Ctrl Pts',(0.0308106631569891,-0.178364693496558,
0.193440144546012));
#20912=CARTESIAN_POINT('Ctrl Pts',(-0.118879635670858,-0.129347344159377,
0.186233046941385));
#20913=CARTESIAN_POINT('Ctrl Pts',(-0.153988624301243,-0.0392836590090855,
0.18161260797309));
#20914=CARTESIAN_POINT('Ctrl Pts',(-0.154326766555531,0.000123460234585825,
0.179578827641127));
#20915=CARTESIAN_POINT('Ctrl Pts',(0.0958116152722397,0.0825211298936481,
0.24));
#20916=CARTESIAN_POINT('Ctrl Pts',(0.122635035163896,0.0513776495479799,
0.237413341363667));
#20917=CARTESIAN_POINT('Ctrl Pts',(0.143215100114593,-0.0385359791949074,
0.232240024091002));
#20918=CARTESIAN_POINT('Ctrl Pts',(0.0482740424593604,-0.140360024672886,
0.224480048182004));
#20919=CARTESIAN_POINT('Ctrl Pts',(-0.0890179591196291,-0.118613269413641,
0.216720072273006));
#20920=CARTESIAN_POINT('Ctrl Pts',(-0.148173729266643,0.00709031985706173,
0.208960096364008));
#20921=CARTESIAN_POINT('Ctrl Pts',(-0.0772398646297824,0.126660050524678,
0.20120012045501));
#20922=CARTESIAN_POINT('Ctrl Pts',(0.0614999571705377,0.134986384232796,
0.193440144546013));
#20923=CARTESIAN_POINT('Ctrl Pts',(0.146250332679645,0.0248320655601208,
0.185680168637014));
#20924=CARTESIAN_POINT('Ctrl Pts',(0.102605431992647,-0.107135610424167,
0.177920192728017));
#20925=CARTESIAN_POINT('Ctrl Pts',(-0.0311170694815965,-0.145041225920327,
0.170160216819019));
#20926=CARTESIAN_POINT('Ctrl Pts',(-0.137521919612742,-0.0556176253575994,
0.162400240910021));
#20927=CARTESIAN_POINT('Ctrl Pts',(-0.123195064154356,0.0826350160503635,
0.154640265001023));
#20928=CARTESIAN_POINT('Ctrl Pts',(-0.000714373963154436,0.148340737886347,
0.146880289092025));
#20929=CARTESIAN_POINT('Ctrl Pts',(0.122393508228972,0.0838174917835845,
0.139120313183027));
#20930=CARTESIAN_POINT('Ctrl Pts',(0.138051156695079,-0.0542900601549481,
0.131360337274029));
#20931=CARTESIAN_POINT('Ctrl Pts',(0.032512624755586,-0.14473579684844,
0.123600361365031));
#20932=CARTESIAN_POINT('Ctrl Pts',(-0.101568992309399,-0.108116932194331,
0.115840385456033));
#20933=CARTESIAN_POINT('Ctrl Pts',(-0.146482409833755,0.0234186855983926,
0.108080409547036));
#20934=CARTESIAN_POINT('Ctrl Pts',(-0.0627977522708403,0.13439480632666,
0.100320433638038));
#20935=CARTESIAN_POINT('Ctrl Pts',(0.076017492057093,0.127384745546031,
0.0925604577290397));
#20936=CARTESIAN_POINT('Ctrl Pts',(0.148096483096158,0.00854251017184644,
0.0848004818200417));
#20937=CARTESIAN_POINT('Ctrl Pts',(0.0901602332714121,-0.117799054254564,
0.0770405059110438));
#20938=CARTESIAN_POINT('Ctrl Pts',(-0.0469280390901857,-0.140724300875114,
0.069280530002046));
#20939=CARTESIAN_POINT('Ctrl Pts',(-0.142818485852497,-0.0401058440029853,
0.0615205540930479));
#20940=CARTESIAN_POINT('Ctrl Pts',(-0.113326201176411,0.0957204333280909,
0.0537605781840501));
#20941=CARTESIAN_POINT('Ctrl Pts',(0.0156536221268617,0.147515686656254,
0.0460006022750521));
#20942=CARTESIAN_POINT('Ctrl Pts',(0.130895613795878,0.0698006416724775,
0.0382406263660543));
#20943=CARTESIAN_POINT('Ctrl Pts',(0.13121455111358,-0.0691831643991777,
0.0304806504570563));
#20944=CARTESIAN_POINT('Ctrl Pts',(0.0163559286405278,-0.147449139316739,
0.0227206745480584));
#20945=CARTESIAN_POINT('Ctrl Pts',(-0.112893560070904,-0.0962328986104914,
0.0149606986390606));
#20946=CARTESIAN_POINT('Ctrl Pts',(-0.142972035491037,0.0393992613429074,
0.00720072273006258));
#20947=CARTESIAN_POINT('Ctrl Pts',(-0.0476516261894416,0.140572551456688,
-0.000559253178935252));
#20948=CARTESIAN_POINT('Ctrl Pts',(0.0897382482543901,0.118078928660352,
-0.00831922908793326));
#20949=CARTESIAN_POINT('Ctrl Pts',(0.128447313976429,0.0343555272840613,
-0.0134925463605985));
#20950=CARTESIAN_POINT('Ctrl Pts',(0.126272937371016,-0.00668937872268922,
-0.0160792049969311));
#20951=CARTESIAN_POINT('Ctrl Pts',(0.102845629995666,0.0885794229410663,
0.245359734998977));
#20952=CARTESIAN_POINT('Ctrl Pts',(0.13163829265517,0.0551495423644061,
0.242773076362644));
#20953=CARTESIAN_POINT('Ctrl Pts',(0.153729244145676,-0.0413651001137901,
0.237599759089979));
#20954=CARTESIAN_POINT('Ctrl Pts',(0.0518180837997932,-0.150664563191773,
0.229839783180981));
#20955=CARTESIAN_POINT('Ctrl Pts',(-0.0955532172229155,-0.127321268762976,
0.222079807271983));
#20956=CARTESIAN_POINT('Ctrl Pts',(-0.159051911315084,0.00761085605850937,
0.214319831362985));
#20957=CARTESIAN_POINT('Ctrl Pts',(-0.0829104333128967,0.135958804728216,
0.206559855453988));
#20958=CARTESIAN_POINT('Ctrl Pts',(0.0660149797280689,0.144896416659008,
0.19879987954499));
#20959=CARTESIAN_POINT('Ctrl Pts',(0.156987308467515,0.0266551129460425,
0.191039903635992));
#20960=CARTESIAN_POINT('Ctrl Pts',(0.110138215124307,-0.11500097684123,
0.183279927726994));
#20961=CARTESIAN_POINT('Ctrl Pts',(-0.0334015307576278,-0.155689435072511,
0.175519951817996));
#20962=CARTESIAN_POINT('Ctrl Pts',(-0.147618098500879,-0.0597007962188336,
0.167759975908998));
#20963=CARTESIAN_POINT('Ctrl Pts',(-0.13223943620312,0.0887016700559064,
0.16));
#20964=CARTESIAN_POINT('Ctrl Pts',(-0.000766819764851659,0.159231180881298,
0.152240024091002));
#20965=CARTESIAN_POINT('Ctrl Pts',(0.131379034007743,0.0899709573066447,
0.144480048182004));
#20966=CARTESIAN_POINT('Ctrl Pts',(0.14818618955117,-0.0582757677477129,
0.136720072273006));
#20967=CARTESIAN_POINT('Ctrl Pts',(0.0348995407947136,-0.15536158290941,
0.128960096364009));
#20968=CARTESIAN_POINT('Ctrl Pts',(-0.109025685167754,-0.116054342400242,
0.12120012045501));
#20969=CARTESIAN_POINT('Ctrl Pts',(-0.157236423577976,0.0251379696208395,
0.113440144546013));
#20970=CARTESIAN_POINT('Ctrl Pts',(-0.0674080525232269,0.144261408030094,
0.105680168637014));
#20971=CARTESIAN_POINT('Ctrl Pts',(0.0815983201941432,0.136736703272292,
0.0979201927280168));
#20972=CARTESIAN_POINT('Ctrl Pts',(0.158968994112971,0.00916965900085902,
0.0901602168190187));
#20973=CARTESIAN_POINT('Ctrl Pts',(0.0967793514910216,-0.126447277955604,
0.0824002409100209));
#20974=CARTESIAN_POINT('Ctrl Pts',(-0.0503732635231939,-0.151055582750353,
0.0746402650010229));
#20975=CARTESIAN_POINT('Ctrl Pts',(-0.15330351242688,-0.0430502166284845,
0.066880289092025));
#20976=CARTESIAN_POINT('Ctrl Pts',(-0.121646050135849,0.102747753924341,
0.0591203131830272));
#20977=CARTESIAN_POINT('Ctrl Pts',(0.0168028336102756,0.158345558472194,
0.0513603372740292));
#20978=CARTESIAN_POINT('Ctrl Pts',(0.140505322097486,0.074925059414875,
0.0436003613650313));
#20979=CARTESIAN_POINT('Ctrl Pts',(0.140847674214973,-0.0742622500154084,
0.0358403854560334));
#20980=CARTESIAN_POINT('Ctrl Pts',(0.0175566999932067,-0.158274125556283,
0.0280804095470355));
#20981=CARTESIAN_POINT('Ctrl Pts',(-0.121181646661057,-0.103297841872129,
0.0203204336380376));
#20982=CARTESIAN_POINT('Ctrl Pts',(-0.153468334920127,0.0422917601656304,
0.0125604577290396));
#20983=CARTESIAN_POINT('Ctrl Pts',(-0.0511499728070136,0.150892692640473,
0.00480048182004178));
#20984=CARTESIAN_POINT('Ctrl Pts',(0.0963263864220051,0.126747699355464,
-0.00295949408895622));
#20985=CARTESIAN_POINT('Ctrl Pts',(0.137877280219327,0.0368777401082635,
-0.00813281136162143));
#20986=CARTESIAN_POINT('Ctrl Pts',(0.135543271642224,-0.00718047980988283,
-0.0107194699979541));
#20987=CARTESIAN_POINT('Ctrl Pts',(0.109879644719093,0.0946377159884845,
0.250719469997954));
#20988=CARTESIAN_POINT('Ctrl Pts',(0.140641550146443,0.0589214351808321,
0.248132811361621));
#20989=CARTESIAN_POINT('Ctrl Pts',(0.164243388176759,-0.0441942210326729,
0.242959494088956));
#20990=CARTESIAN_POINT('Ctrl Pts',(0.055362125140226,-0.160969101710661,
0.235199518179958));
#20991=CARTESIAN_POINT('Ctrl Pts',(-0.102088475326202,-0.13602926811231,
0.227439542270961));
#20992=CARTESIAN_POINT('Ctrl Pts',(-0.169930093363525,0.00813139225995705,
0.219679566361962));
#20993=CARTESIAN_POINT('Ctrl Pts',(-0.0885810019960112,0.145257558931755,
0.211919590452965));
#20994=CARTESIAN_POINT('Ctrl Pts',(0.0705300022856002,0.154806449085219,
0.204159614543967));
#20995=CARTESIAN_POINT('Ctrl Pts',(0.167724284255384,0.0284781603319641,
0.196399638634969));
#20996=CARTESIAN_POINT('Ctrl Pts',(0.117670998255967,-0.122866343258294,
0.188639662725971));
#20997=CARTESIAN_POINT('Ctrl Pts',(-0.0356859920336591,-0.166337644224695,
0.180879686816973));
#20998=CARTESIAN_POINT('Ctrl Pts',(-0.157714277389017,-0.0637839670800676,
0.173119710907975));
#20999=CARTESIAN_POINT('Ctrl Pts',(-0.141283808251885,0.0947683240614489,
0.165359734998977));
#21000=CARTESIAN_POINT('Ctrl Pts',(-0.000819265566548849,0.17012162387625,
0.157599759089979));
#21001=CARTESIAN_POINT('Ctrl Pts',(0.140364559786514,0.0961244228297045,
0.149839783180981));
#21002=CARTESIAN_POINT('Ctrl Pts',(0.158321222407261,-0.0622614753404775,
0.142079807271983));
#21003=CARTESIAN_POINT('Ctrl Pts',(0.0372864568338413,-0.16598736897038,
0.134319831362986));
#21004=CARTESIAN_POINT('Ctrl Pts',(-0.116482378026109,-0.123991752606152,
0.126559855453987));
#21005=CARTESIAN_POINT('Ctrl Pts',(-0.167990437322196,0.0268572536432864,
0.11879987954499));
#21006=CARTESIAN_POINT('Ctrl Pts',(-0.0720183527756138,0.154128009733527,
0.111039903635992));
#21007=CARTESIAN_POINT('Ctrl Pts',(0.0871791483311938,0.146088660998552,
0.103279927726994));
#21008=CARTESIAN_POINT('Ctrl Pts',(0.169841505129784,0.00979680782987164,
0.0955199518179957));
#21009=CARTESIAN_POINT('Ctrl Pts',(0.103398469710631,-0.135095501656644,
0.0877599759089979));
#21010=CARTESIAN_POINT('Ctrl Pts',(-0.0538184879562023,-0.161386864625592,
0.08));
#21011=CARTESIAN_POINT('Ctrl Pts',(-0.163788539001263,-0.0459945892539838,
0.0722400240910021));
#21012=CARTESIAN_POINT('Ctrl Pts',(-0.129965899095288,0.10977507452059,
0.0644800481820042));
#21013=CARTESIAN_POINT('Ctrl Pts',(0.0179520450936897,0.169175430288133,
0.0567200722730062));
#21014=CARTESIAN_POINT('Ctrl Pts',(0.150115030399095,0.0800494771572726,
0.0489600963640084));
#21015=CARTESIAN_POINT('Ctrl Pts',(0.150480797316365,-0.0793413356316391,
0.0412001204550104));
#21016=CARTESIAN_POINT('Ctrl Pts',(0.0187574713458855,-0.169099111795828,
0.0334401445460125));
#21017=CARTESIAN_POINT('Ctrl Pts',(-0.129469733251211,-0.110362785133767,
0.0256801686370146));
#21018=CARTESIAN_POINT('Ctrl Pts',(-0.163964634349217,0.0451842589883535,
0.0179201927280167));
#21019=CARTESIAN_POINT('Ctrl Pts',(-0.0546483194245858,0.161212833824257,
0.0101602168190188));
#21020=CARTESIAN_POINT('Ctrl Pts',(0.10291452458962,0.135416470050577,0.00240024091002082));
#21021=CARTESIAN_POINT('Ctrl Pts',(0.147307246462226,0.0393999529324658,
-0.00277307636264439));
#21022=CARTESIAN_POINT('Ctrl Pts',(0.144813605913432,-0.00767158089707644,
-0.00535973499897704));
#21023=CARTESIAN_POINT('Ctrl Pts',(0.116913659442519,0.100696009035903,
0.256079204996931));
#21024=CARTESIAN_POINT('Ctrl Pts',(0.149644807637716,0.0626933279972582,
0.253492546360598));
#21025=CARTESIAN_POINT('Ctrl Pts',(0.174757532207842,-0.0470233419515556,
0.248319229087933));
#21026=CARTESIAN_POINT('Ctrl Pts',(0.0589061664806588,-0.171273640229548,
0.240559253178935));
#21027=CARTESIAN_POINT('Ctrl Pts',(-0.108623733429488,-0.144737267461644,
0.232799277269938));
#21028=CARTESIAN_POINT('Ctrl Pts',(-0.180808275411966,0.00865192846140473,
0.225039301360939));
#21029=CARTESIAN_POINT('Ctrl Pts',(-0.0942515706791253,0.154556313135293,
0.217279325451942));
#21030=CARTESIAN_POINT('Ctrl Pts',(0.0750450248431312,0.164716481511431,
0.209519349542944));
#21031=CARTESIAN_POINT('Ctrl Pts',(0.178461260043253,0.0303012077178856,
0.201759373633945));
#21032=CARTESIAN_POINT('Ctrl Pts',(0.125203781387627,-0.130731709675357,
0.193999397724948));
#21033=CARTESIAN_POINT('Ctrl Pts',(-0.0379704533096903,-0.17698585337688,
0.18623942181595));
#21034=CARTESIAN_POINT('Ctrl Pts',(-0.167810456277154,-0.0678671379413016,
0.178479445906952));
#21035=CARTESIAN_POINT('Ctrl Pts',(-0.150328180300649,0.100834978066992,
0.170719469997954));
#21036=CARTESIAN_POINT('Ctrl Pts',(-0.000871711368246156,0.181012066871201,
0.162959494088956));
#21037=CARTESIAN_POINT('Ctrl Pts',(0.149350085565286,0.102277888352765,
0.155199518179958));
#21038=CARTESIAN_POINT('Ctrl Pts',(0.168456255263351,-0.0662471829332422,
0.14743954227096));
#21039=CARTESIAN_POINT('Ctrl Pts',(0.0396733728729688,-0.17661315503135,
0.139679566361963));
#21040=CARTESIAN_POINT('Ctrl Pts',(-0.123939070884463,-0.131929162812062,
0.131919590452964));
#21041=CARTESIAN_POINT('Ctrl Pts',(-0.178744451066417,0.0285765376657333,
0.124159614543967));
#21042=CARTESIAN_POINT('Ctrl Pts',(-0.0766286530280003,0.163994611436961,
0.116399638634969));
#21043=CARTESIAN_POINT('Ctrl Pts',(0.0927599764682439,0.155440618724813,
0.108639662725971));
#21044=CARTESIAN_POINT('Ctrl Pts',(0.180714016146597,0.0104239566588842,
0.100879686816973));
#21045=CARTESIAN_POINT('Ctrl Pts',(0.11001758793024,-0.143743725357685,
0.093119710907975));
#21046=CARTESIAN_POINT('Ctrl Pts',(-0.0572637123892103,-0.171718146500831,
0.0853597349989769));
#21047=CARTESIAN_POINT('Ctrl Pts',(-0.174273565575645,-0.048938961879483,
0.0775997590899791));
#21048=CARTESIAN_POINT('Ctrl Pts',(-0.138285748054726,0.11680239511684,
0.0698397831809812));
#21049=CARTESIAN_POINT('Ctrl Pts',(0.0191012565771036,0.180005302104073,
0.0620798072719832));
#21050=CARTESIAN_POINT('Ctrl Pts',(0.159724738700703,0.0851738948996701,
0.0543198313629854));
#21051=CARTESIAN_POINT('Ctrl Pts',(0.160113920417758,-0.0844204212478698,
0.0465598554539874));
#21052=CARTESIAN_POINT('Ctrl Pts',(0.0199582426985643,-0.179924098035372,
0.0387998795449896));
#21053=CARTESIAN_POINT('Ctrl Pts',(-0.137757819841364,-0.117427728395404,
0.0310399036359917));
#21054=CARTESIAN_POINT('Ctrl Pts',(-0.174460933778308,0.0480767578110765,
0.0232799277269937));
#21055=CARTESIAN_POINT('Ctrl Pts',(-0.0581466660421577,0.171532975008042,
0.0155199518179959));
#21056=CARTESIAN_POINT('Ctrl Pts',(0.109502662757235,0.144085240745689,
0.00775997590899784));
#21057=CARTESIAN_POINT('Ctrl Pts',(0.156737212705124,0.0419221657566679,
0.00258665863633264));
#21058=CARTESIAN_POINT('Ctrl Pts',(0.15408394018464,-0.00816268198427004,
0.));
#21059=CARTESIAN_POINT('Ctrl Pts',(0.15408394018464,-0.00816268198427004,
0.));
#21060=CARTESIAN_POINT('Ctrl Pts',(0.153697863146473,0.00250812953454787,
1.45220469349306E-17));
#21061=CARTESIAN_POINT('Ctrl Pts',(0.152123106309386,0.0130673133993916,
-2.32988231788825E-17));
#21062=CARTESIAN_POINT('Ctrl Pts',(0.149466152202855,0.0233620190894148,
-6.07153216591882E-17));
#21063=CARTESIAN_POINT('Ctrl Pts',(0.14793019248835,0.0293132898222067,
-8.23454409684948E-17));
#21064=CARTESIAN_POINT('Ctrl Pts',(0.146031563681721,0.0351760135160456,
3.17823908273165E-17));
#21065=CARTESIAN_POINT('Ctrl Pts',(0.143784059453749,0.0409171473780902,
6.24500451351651E-17));
#21066=CARTESIAN_POINT('Ctrl Pts',(0.142595904075608,0.0439522291322952,
7.86626679846993E-17));
#21067=CARTESIAN_POINT('Ctrl Pts',(0.141309213132582,0.0469553015723855,
1.03399090950918E-16));
#21068=CARTESIAN_POINT('Ctrl Pts',(0.13992871365498,0.0499144025840292,
1.00613961606655E-16));
#21069=CARTESIAN_POINT('Ctrl Pts',(0.135493978469587,0.0594202586791481,
9.16669744478229E-17));
#21070=CARTESIAN_POINT('Ctrl Pts',(0.130119641392827,0.0684241765595774,
5.76730757846686E-17));
#21071=CARTESIAN_POINT('Ctrl Pts',(0.123887660540245,0.0767683201192124,
1.38777878078145E-16));
#21072=CARTESIAN_POINT('Ctrl Pts',(0.120656388342022,0.0810947453345699,
1.808305895663E-16));
#21073=CARTESIAN_POINT('Ctrl Pts',(0.117193874983239,0.0852432898306738,
1.062697842984E-16));
#21074=CARTESIAN_POINT('Ctrl Pts',(0.11350808038867,0.0891875047540603,
1.14491749414469E-16));
#21075=CARTESIAN_POINT('Ctrl Pts',(0.110158526423333,0.0927719043720516,
1.21963656801269E-16));
#21076=CARTESIAN_POINT('Ctrl Pts',(0.106618991420749,0.0961915975683434,
1.17223950247179E-16));
#21077=CARTESIAN_POINT('Ctrl Pts',(0.102922970874274,0.0994011657423757,
1.02348685082632E-16));
#21078=CARTESIAN_POINT('Ctrl Pts',(0.0973787571548163,0.104215676830788,
8.00350512245867E-17));
#21079=CARTESIAN_POINT('Ctrl Pts',(0.0914754811895955,0.108568278221023,
6.56075743842472E-17));
#21080=CARTESIAN_POINT('Ctrl Pts',(0.0852365492443714,0.11239450959967,
3.29597460435593E-17));
#21081=CARTESIAN_POINT('Ctrl Pts',(0.0787787796913796,0.116354950379705,
-7.26807264206779E-19));
#21082=CARTESIAN_POINT('Ctrl Pts',(0.0719608771003193,0.11975150351845,
7.81983513604452E-17));
#21083=CARTESIAN_POINT('Ctrl Pts',(0.0648645680501024,0.122569786811788,
1.05818132034585E-16));
#21084=CARTESIAN_POINT('Ctrl Pts',(0.0619760396963809,0.123716959397427,
1.17060669392563E-16));
#21085=CARTESIAN_POINT('Ctrl Pts',(0.0590419697559043,0.124767587801255,
-1.70921410850511E-17));
#21086=CARTESIAN_POINT('Ctrl Pts',(0.0560804949635964,0.12571697313192,
-8.67361737988404E-19));
#21087=CARTESIAN_POINT('Ctrl Pts',(0.0481895916857994,0.128246627558523,
4.23638569993146E-17));
#21088=CARTESIAN_POINT('Ctrl Pts',(0.040081547172159,0.13006877931966,2.48189907303608E-17));
#21089=CARTESIAN_POINT('Ctrl Pts',(0.0318655688619291,0.131172622122806,
0.));
#21090=CARTESIAN_POINT('Ctrl Pts',(0.0267717292715239,0.131856995664207,
-1.5387571972871E-17));
#21091=CARTESIAN_POINT('Ctrl Pts',(0.0216363184326117,0.132264755542675,
5.61228976213782E-17));
#21092=CARTESIAN_POINT('Ctrl Pts',(0.0164863123329273,0.132388468809724,
3.03576608295941E-17));
#21093=CARTESIAN_POINT('Ctrl Pts',(0.0120733572364389,0.13249447666326,
8.27985532573229E-18));
#21094=CARTESIAN_POINT('Ctrl Pts',(0.00764667637530932,0.132391154756805,
7.9933444120104E-17));
#21095=CARTESIAN_POINT('Ctrl Pts',(0.00324855819595315,0.132074892239241,
9.62771529167128E-17));
#21096=CARTESIAN_POINT('Ctrl Pts',(-0.00215998367955725,0.131685971569047,
1.16375665467493E-16));
#21097=CARTESIAN_POINT('Ctrl Pts',(-0.00753310453775717,0.130975837616781,
1.12286849362194E-16));
#21098=CARTESIAN_POINT('Ctrl Pts',(-0.0128378223015392,0.129936202211006,
1.27068494615301E-16));
#21099=CARTESIAN_POINT('Ctrl Pts',(-0.0180922709275414,0.128906418710228,
1.41710064449709E-16));
#21100=CARTESIAN_POINT('Ctrl Pts',(-0.023283936630727,0.12755123862641,
1.19281234835921E-16));
#21101=CARTESIAN_POINT('Ctrl Pts',(-0.028350637156304,0.125868914531291,
9.19403442267708E-17));
#21102=CARTESIAN_POINT('Ctrl Pts',(-0.0326437071621008,0.124443463179602,
6.87741127091605E-17));
#21103=CARTESIAN_POINT('Ctrl Pts',(-0.0368509055758185,0.122782751372096,
3.08039683582783E-17));
#21104=CARTESIAN_POINT('Ctrl Pts',(-0.0409513668396969,0.120880349084932,
-1.95156391047391E-18));
#21105=CARTESIAN_POINT('Ctrl Pts',(-0.0436523616789034,0.119627226953286,
-2.45035827619675E-17));
#21106=CARTESIAN_POINT('Ctrl Pts',(-0.0463070048384274,0.118269169850402,
-4.56986185075063E-18));
#21107=CARTESIAN_POINT('Ctrl Pts',(-0.0489111879062984,0.116810626195002,
-1.73472347597681E-18));
#21108=CARTESIAN_POINT('Ctrl Pts',(0.0958116152722397,0.0825211298936481,
0.24));
#21109=CARTESIAN_POINT('Ctrl Pts',(0.102494250906434,0.0762804363331629,
0.24));
#21110=CARTESIAN_POINT('Ctrl Pts',(0.108399952301676,0.0693089192431419,
0.24));
#21111=CARTESIAN_POINT('Ctrl Pts',(0.113520383394708,0.0617855200816623,
0.24));
#21112=CARTESIAN_POINT('Ctrl Pts',(0.11760088593285,0.0557900777417299,
0.24));
#21113=CARTESIAN_POINT('Ctrl Pts',(0.1211824537664,0.0494427873910869,0.24));
#21114=CARTESIAN_POINT('Ctrl Pts',(0.124247292533427,0.0428169095598754,
0.24));
#21115=CARTESIAN_POINT('Ctrl Pts',(0.125635784531567,0.0398151273949318,
0.24));
#21116=CARTESIAN_POINT('Ctrl Pts',(0.126914357096627,0.0367636074968772,
0.24));
#21117=CARTESIAN_POINT('Ctrl Pts',(0.128080244072735,0.0336751552254939,
0.24));
#21118=CARTESIAN_POINT('Ctrl Pts',(0.13155694143068,0.024465331227027,0.24));
#21119=CARTESIAN_POINT('Ctrl Pts',(0.134041462136676,0.0149150332268467,
0.24));
#21120=CARTESIAN_POINT('Ctrl Pts',(0.135496608205084,0.00520422800883078,
0.24));
#21121=CARTESIAN_POINT('Ctrl Pts',(0.136052940597398,0.00149158663520877,
0.24));
#21122=CARTESIAN_POINT('Ctrl Pts',(0.136458356591543,-0.00224482315054724,
0.24));
#21123=CARTESIAN_POINT('Ctrl Pts',(0.136708928272429,-0.00599574054845843,
0.24));
#21124=CARTESIAN_POINT('Ctrl Pts',(0.136894600108428,-0.00877514370161729,
0.24));
#21125=CARTESIAN_POINT('Ctrl Pts',(0.136994942037659,-0.0115613689854128,
0.24));
#21126=CARTESIAN_POINT('Ctrl Pts',(0.137008733057845,-0.0143405417274864,
0.24));
#21127=CARTESIAN_POINT('Ctrl Pts',(0.137045731231951,-0.0217964308202384,
0.24));
#21128=CARTESIAN_POINT('Ctrl Pts',(0.136462408227525,-0.0292204075226799,
0.24));
#21129=CARTESIAN_POINT('Ctrl Pts',(0.135240454646173,-0.0365388974416549,
0.24));
#21130=CARTESIAN_POINT('Ctrl Pts',(0.134058793448489,-0.0436160693529878,
0.24));
#21131=CARTESIAN_POINT('Ctrl Pts',(0.132280018312676,-0.050595007513092,
0.24));
#21132=CARTESIAN_POINT('Ctrl Pts',(0.129952822193542,-0.0574290655609092,
0.24));
#21133=CARTESIAN_POINT('Ctrl Pts',(0.128850070284018,-0.0606674134165377,
0.24));
#21134=CARTESIAN_POINT('Ctrl Pts',(0.127623182384127,-0.0638741644409745,
0.24));
#21135=CARTESIAN_POINT('Ctrl Pts',(0.126284110088584,-0.067028198101918,
0.24));
#21136=CARTESIAN_POINT('Ctrl Pts',(0.122654675969015,-0.0755769205431157,
0.24));
#21137=CARTESIAN_POINT('Ctrl Pts',(0.118195290975453,-0.0837663478860722,
0.24));
#21138=CARTESIAN_POINT('Ctrl Pts',(0.113014989178579,-0.0915013065162071,
0.24));
#21139=CARTESIAN_POINT('Ctrl Pts',(0.108985931714537,-0.0975172866704144,
0.24));
#21140=CARTESIAN_POINT('Ctrl Pts',(0.104519884911976,-0.103258562704539,
0.24));
#21141=CARTESIAN_POINT('Ctrl Pts',(0.0996546828651377,-0.108675969178894,
0.24));
#21142=CARTESIAN_POINT('Ctrl Pts',(0.0972822643803542,-0.11131765910988,
0.24));
#21143=CARTESIAN_POINT('Ctrl Pts',(0.09482095240722,-0.113875293456495,
0.24));
#21144=CARTESIAN_POINT('Ctrl Pts',(0.0922773332174137,-0.116342466058553,
0.24));
#21145=CARTESIAN_POINT('Ctrl Pts',(0.0868426048671788,-0.121613857680014,
0.24));
#21146=CARTESIAN_POINT('Ctrl Pts',(0.0810310485854155,-0.126474759557936,
0.24));
#21147=CARTESIAN_POINT('Ctrl Pts',(0.0748870600798396,-0.130870957562724,
0.24));
#21148=CARTESIAN_POINT('Ctrl Pts',(0.0715378781224404,-0.133267392228159,
0.24));
#21149=CARTESIAN_POINT('Ctrl Pts',(0.0680912231566627,-0.135524142754832,
0.24));
#21150=CARTESIAN_POINT('Ctrl Pts',(0.0645638484115253,-0.13762659390894,
0.24));
#21151=CARTESIAN_POINT('Ctrl Pts',(0.0598451535113139,-0.140439117742,0.24));
#21152=CARTESIAN_POINT('Ctrl Pts',(0.0549775790306604,-0.142978967531553,
0.24));
#21153=CARTESIAN_POINT('Ctrl Pts',(0.0499773507040556,-0.145225083935062,
0.24));
#21154=CARTESIAN_POINT('Ctrl Pts',(0.0466920976074369,-0.146700828718701,
0.24));
#21155=CARTESIAN_POINT('Ctrl Pts',(0.0433495270099635,-0.148049731670784,
0.24));
#21156=CARTESIAN_POINT('Ctrl Pts',(0.039956549802796,-0.149273502906639,
0.24));
#21157=CARTESIAN_POINT('Ctrl Pts',(-0.126296536029262,-6.10717992316628E-5,
0.159341967361942));
#21158=CARTESIAN_POINT('Ctrl Pts',(-0.12637083907321,-0.0163056929409037,
0.160361391877968));
#21159=CARTESIAN_POINT('Ctrl Pts',(-0.12344809088261,-0.0325245895549842,
0.161380816393994));
#21160=CARTESIAN_POINT('Ctrl Pts',(-0.117399968681154,-0.0474794518833934,
0.162400240910021));
#21161=CARTESIAN_POINT('Ctrl Pts',(-0.102053636235694,-0.0854254922118417,
0.164986899546353));
#21162=CARTESIAN_POINT('Ctrl Pts',(-0.0665853528586453,-0.115233359066084,
0.167573558182686));
#21163=CARTESIAN_POINT('Ctrl Pts',(-0.0265641275910804,-0.123819689910512,
0.170160216819019));
#21164=CARTESIAN_POINT('Ctrl Pts',(0.0134570976764845,-0.13240602075494,
0.172746875455351));
#21165=CARTESIAN_POINT('Ctrl Pts',(0.058031264834566,-0.119770815589554,
0.175333534091684));
#21166=CARTESIAN_POINT('Ctrl Pts',(0.0875924985281064,-0.0914586003428122,
0.177920192728017));
#21167=CARTESIAN_POINT('Ctrl Pts',(0.117153732221647,-0.0631463850960709,
0.180506851364349));
#21168=CARTESIAN_POINT('Ctrl Pts',(0.131702032450646,-0.0191571597679751,
0.183093510000682));
#21169=CARTESIAN_POINT('Ctrl Pts',(0.124851119980295,0.0211965060081854,
0.185680168637015));
#21170=CARTESIAN_POINT('Ctrl Pts',(0.118000207509943,0.0615501717843459,
0.188266827273347));
#21171=CARTESIAN_POINT('Ctrl Pts',(0.0897500823402403,0.0982682780085711,
0.19085348590968));
#21172=CARTESIAN_POINT('Ctrl Pts',(0.0525017161220023,0.115239608835997,
0.193440144546013));
#21173=CARTESIAN_POINT('Ctrl Pts',(0.0152533499037644,0.132210939663423,
0.196026803182345));
#21174=CARTESIAN_POINT('Ctrl Pts',(-0.030993257363009,0.129435495094051,
0.198613461818678));
#21175=CARTESIAN_POINT('Ctrl Pts',(-0.0659388717692058,0.108119484364762,
0.20120012045501));
#21176=CARTESIAN_POINT('Ctrl Pts',(-0.100884486175403,0.0868034736354726,
0.203786779091343));
#21177=CARTESIAN_POINT('Ctrl Pts',(-0.124529107721023,0.0469468967462671,
0.206373437727676));
#21178=CARTESIAN_POINT('Ctrl Pts',(-0.126492123469331,0.00606801008988057,
0.208960096364008));
#21179=CARTESIAN_POINT('Ctrl Pts',(-0.126588724127832,0.00405634646811867,
0.209087386696653));
#21180=CARTESIAN_POINT('Ctrl Pts',(-0.126632819376787,0.00204220716288977,
0.209214677029297));
#21181=CARTESIAN_POINT('Ctrl Pts',(-0.126625441102054,2.7778768752873E-5,
0.209341967361942));
#21182=CARTESIAN_POINT('Ctrl Pts',(-0.0398513841857245,-0.149064942821851,
0.24));
#21183=CARTESIAN_POINT('Ctrl Pts',(-0.0883048112969314,-0.136111285829332,
0.237413341363667));
#21184=CARTESIAN_POINT('Ctrl Pts',(-0.170871437255804,-0.0596187094618861,
0.232240024091002));
#21185=CARTESIAN_POINT('Ctrl Pts',(-0.145169204726118,0.108307533342445,
0.224480048182004));
#21186=CARTESIAN_POINT('Ctrl Pts',(0.00818767200092134,0.180778621679153,
0.216720072273006));
#21187=CARTESIAN_POINT('Ctrl Pts',(0.154249898498561,0.0947283641859207,
0.208960096364008));
#21188=CARTESIAN_POINT('Ctrl Pts',(0.164950538597243,-0.0745810526211722,
0.201200120455011));
#21189=CARTESIAN_POINT('Ctrl Pts',(0.0308106631569891,-0.178364693496558,
0.193440144546012));
#21190=CARTESIAN_POINT('Ctrl Pts',(-0.13036283225522,-0.125587074703769,
0.185680168637015));
#21191=CARTESIAN_POINT('Ctrl Pts',(-0.17709781441264,0.03745832727601,0.177920192728017));
#21192=CARTESIAN_POINT('Ctrl Pts',(-0.0683530255288039,0.167611467503216,
0.170160216819019));
#21193=CARTESIAN_POINT('Ctrl Pts',(0.100397202365132,0.150621028353064,
0.162400240910021));
#21194=CARTESIAN_POINT('Ctrl Pts',(0.18100910679194,0.00139719974911195,
0.154640265001023));
#21195=CARTESIAN_POINT('Ctrl Pts',(0.102711092909207,-0.149052183789333,
0.146880289092025));
#21196=CARTESIAN_POINT('Ctrl Pts',(-0.0657574679958034,-0.168648048308422,
0.139120313183027));
#21197=CARTESIAN_POINT('Ctrl Pts',(-0.176497206835689,-0.0401861834345609,
0.131360337274029));
#21198=CARTESIAN_POINT('Ctrl Pts',(-0.132288575936487,0.123555290563421,
0.123600361365031));
#21199=CARTESIAN_POINT('Ctrl Pts',(0.0280571680938306,0.178826694862324,
0.115840385456033));
#21200=CARTESIAN_POINT('Ctrl Pts',(0.163771354656592,0.0771047007047774,
0.108080409547035));
#21201=CARTESIAN_POINT('Ctrl Pts',(0.155709331479018,-0.0923080778690166,
0.100320433638038));
#21202=CARTESIAN_POINT('Ctrl Pts',(0.0109489686262093,-0.180682908560435,
0.0925604577290397));
#21203=CARTESIAN_POINT('Ctrl Pts',(-0.143423754439364,-0.110434756566834,
0.0848004818200417));
#21204=CARTESIAN_POINT('Ctrl Pts',(-0.17188331593326,0.0567648465404429,
0.0770405059110439));
#21205=CARTESIAN_POINT('Ctrl Pts',(-0.0494457976037486,0.174130301808973,
0.0692805300020459));
#21206=CARTESIAN_POINT('Ctrl Pts',(0.11640175885633,0.13862511662766,0.061520554093048));
#21207=CARTESIAN_POINT('Ctrl Pts',(0.18005704388064,-0.0185795878987759,
0.0537605781840501));
#21208=CARTESIAN_POINT('Ctrl Pts',(0.0856431484406112,-0.159474177462153,
0.0460006022750521));
#21209=CARTESIAN_POINT('Ctrl Pts',(-0.0839657292871194,-0.160363143120653,
0.0382406263660544));
#21210=CARTESIAN_POINT('Ctrl Pts',(-0.179844832231877,-0.0204718628801216,
0.0304806504570563));
#21211=CARTESIAN_POINT('Ctrl Pts',(-0.117866479118068,0.137399078213474,
0.0227206745480585));
#21212=CARTESIAN_POINT('Ctrl Pts',(0.0476444145610997,0.174632482457551,
0.0149606986390605));
#21213=CARTESIAN_POINT('Ctrl Pts',(0.171219786572432,0.0585809927800803,
0.00720072273006264));
#21214=CARTESIAN_POINT('Ctrl Pts',(0.144688050375066,-0.108949473877577,
-0.000559253178935319));
#21215=CARTESIAN_POINT('Ctrl Pts',(-0.0092814439579932,-0.180735423716049,
-0.00831922908793317));
#21216=CARTESIAN_POINT('Ctrl Pts',(-0.105867686800049,-0.122947365648507,
-0.0134925463605985));
#21217=CARTESIAN_POINT('Ctrl Pts',(-0.131895903200816,-0.0800747195988904,
-0.0160792049969312));
#21218=CARTESIAN_POINT('Ctrl Pts',(-0.0374537582415196,-0.140096572423086,
0.245359734998977));
#21219=CARTESIAN_POINT('Ctrl Pts',(-0.0829920245295529,-0.127922261611689,
0.242773076362644));
#21220=CARTESIAN_POINT('Ctrl Pts',(-0.160591096949962,-0.0560317985556137,
0.237599759089979));
#21221=CARTESIAN_POINT('Ctrl Pts',(-0.13643521822445,0.101791299158848,
0.229839783180981));
#21222=CARTESIAN_POINT('Ctrl Pts',(0.00769506740980954,0.1699022237233,
0.222079807271983));
#21223=CARTESIAN_POINT('Ctrl Pts',(0.144969579481095,0.0890291096113304,
0.214319831362985));
#21224=CARTESIAN_POINT('Ctrl Pts',(0.155026424317845,-0.0700939445729984,
0.206559855453987));
#21225=CARTESIAN_POINT('Ctrl Pts',(0.0289569648011409,-0.167633527556011,
0.19879987954499));
#21226=CARTESIAN_POINT('Ctrl Pts',(-0.122519659046519,-0.118031231043151,
0.191039903635991));
#21227=CARTESIAN_POINT('Ctrl Pts',(-0.166442869216287,0.0352046776440443,
0.183279927726994));
#21228=CARTESIAN_POINT('Ctrl Pts',(-0.064240621638164,0.157527260611955,
0.175519951817996));
#21229=CARTESIAN_POINT('Ctrl Pts',(0.0943568867767351,0.141559037340679,
0.167759975908998));
#21230=CARTESIAN_POINT('Ctrl Pts',(0.170118841887737,0.00131313836865665,
0.16));
#21231=CARTESIAN_POINT('Ctrl Pts',(0.0965315639882279,-0.140084581027326,
0.152240024091002));
#21232=CARTESIAN_POINT('Ctrl Pts',(-0.0618012237018238,-0.158501476380598,
0.144480048182004));
#21233=CARTESIAN_POINT('Ctrl Pts',(-0.165878396703103,-0.0377684145673052,
0.136720072273006));
#21234=CARTESIAN_POINT('Ctrl Pts',(-0.124329541933827,0.116121687534276,
0.128960096364008));
#21235=CARTESIAN_POINT('Ctrl Pts',(0.0263691315170036,0.168067732987372,
0.12120012045501));
#21236=CARTESIAN_POINT('Ctrl Pts',(0.153918185014798,0.0724657594331675,
0.113440144546012));
#21237=CARTESIAN_POINT('Ctrl Pts',(0.146341206869619,-0.0867544378416841,
0.105680168637015));
#21238=CARTESIAN_POINT('Ctrl Pts',(0.0102902328814698,-0.169812269106107,
0.0979201927280167));
#21239=CARTESIAN_POINT('Ctrl Pts',(-0.134794781526993,-0.103790539737311,
0.0901602168190187));
#21240=CARTESIAN_POINT('Ctrl Pts',(-0.161542096774173,0.0533496359633175,
0.0824002409100209));
#21241=CARTESIAN_POINT('Ctrl Pts',(-0.0464709316213242,0.163653894581969,
0.074640265001023));
#21242=CARTESIAN_POINT('Ctrl Pts',(0.109398542213106,0.130284849835523,
0.066880289092025));
#21243=CARTESIAN_POINT('Ctrl Pts',(0.16922405906302,-0.0174617621848401,
0.0591203131830272));
#21244=CARTESIAN_POINT('Ctrl Pts',(0.0804904984426183,-0.149879543972585,
0.0513603372740291));
#21245=CARTESIAN_POINT('Ctrl Pts',(-0.0789139998409189,-0.150715025739123,
0.0436003613650314));
#21246=CARTESIAN_POINT('Ctrl Pts',(-0.169024614954586,-0.0192401899891918,
0.0358403854560333));
#21247=CARTESIAN_POINT('Ctrl Pts',(-0.110775138777956,0.12913257502003,
0.0280804095470356));
#21248=CARTESIAN_POINT('Ctrl Pts',(0.0447779273164969,0.164125861942445,
0.0203204336380375));
#21249=CARTESIAN_POINT('Ctrl Pts',(0.16091848811479,0.0550565152494576,
0.0125604577290397));
#21250=CARTESIAN_POINT('Ctrl Pts',(0.135983012131502,-0.10239461786658,
0.00480048182004171));
#21251=CARTESIAN_POINT('Ctrl Pts',(-0.00872303347143,-0.169861624730324,
-0.00295949408895612));
#21252=CARTESIAN_POINT('Ctrl Pts',(-0.0994982439886826,-0.115550337924785,
-0.00813281136162148));
#21253=CARTESIAN_POINT('Ctrl Pts',(-0.123960494032221,-0.0752570895690155,
-0.0107194699979541));
#21254=CARTESIAN_POINT('Ctrl Pts',(-0.0350561322973148,-0.13112820202432,
0.250719469997954));
#21255=CARTESIAN_POINT('Ctrl Pts',(-0.0776792377621743,-0.119733237394047,
0.248132811361621));
#21256=CARTESIAN_POINT('Ctrl Pts',(-0.150310756644121,-0.0524448876493412,
0.242959494088956));
#21257=CARTESIAN_POINT('Ctrl Pts',(-0.127701231722781,0.0952750649752511,
0.235199518179958));
#21258=CARTESIAN_POINT('Ctrl Pts',(0.00720246281869772,0.159025825767447,
0.22743954227096));
#21259=CARTESIAN_POINT('Ctrl Pts',(0.135689260463629,0.08332985503674,0.219679566361962));
#21260=CARTESIAN_POINT('Ctrl Pts',(0.145102310038447,-0.0656068365248246,
0.211919590452964));
#21261=CARTESIAN_POINT('Ctrl Pts',(0.0271032664452926,-0.156902361615465,
0.204159614543967));
#21262=CARTESIAN_POINT('Ctrl Pts',(-0.114676485837817,-0.110475387382534,
0.196399638634969));
#21263=CARTESIAN_POINT('Ctrl Pts',(-0.155787924019933,0.0329510280120788,
0.188639662725971));
#21264=CARTESIAN_POINT('Ctrl Pts',(-0.0601282177475243,0.147443053720694,
0.180879686816973));
#21265=CARTESIAN_POINT('Ctrl Pts',(0.0883165711883383,0.132497046328295,
0.173119710907975));
#21266=CARTESIAN_POINT('Ctrl Pts',(0.159228576983534,0.00122907698820117,
0.165359734998977));
#21267=CARTESIAN_POINT('Ctrl Pts',(0.0903520350672485,-0.131116978265319,
0.157599759089979));
#21268=CARTESIAN_POINT('Ctrl Pts',(-0.0578449794078444,-0.148354904452775,
0.149839783180981));
#21269=CARTESIAN_POINT('Ctrl Pts',(-0.155259586570517,-0.0353506457000499,
0.142079807271983));
#21270=CARTESIAN_POINT('Ctrl Pts',(-0.116370507931168,0.108688084505131,
0.134319831362985));
#21271=CARTESIAN_POINT('Ctrl Pts',(0.0246810949401768,0.157308771112418,
0.126559855453988));
#21272=CARTESIAN_POINT('Ctrl Pts',(0.144065015373005,0.0678268181615582,
0.118799879544989));
#21273=CARTESIAN_POINT('Ctrl Pts',(0.13697308226022,-0.0812007978143519,
0.111039903635992));
#21274=CARTESIAN_POINT('Ctrl Pts',(0.00963149713673027,-0.15894162965178,
0.103279927726994));
#21275=CARTESIAN_POINT('Ctrl Pts',(-0.126165808614623,-0.0971463229077874,
0.0955199518179957));
#21276=CARTESIAN_POINT('Ctrl Pts',(-0.151200877615086,0.0499344253861922,
0.087759975908998));
#21277=CARTESIAN_POINT('Ctrl Pts',(-0.0434960656388994,0.153177487354966,
0.08));
#21278=CARTESIAN_POINT('Ctrl Pts',(0.102395325569881,0.121944583043386,
0.072240024091002));
#21279=CARTESIAN_POINT('Ctrl Pts',(0.158391074245402,-0.0163439364709043,
0.0644800481820042));
#21280=CARTESIAN_POINT('Ctrl Pts',(0.0753378484446251,-0.140284910483017,
0.0567200722730062));
#21281=CARTESIAN_POINT('Ctrl Pts',(-0.0738622703947183,-0.141066908357593,
0.0489600963640083));
#21282=CARTESIAN_POINT('Ctrl Pts',(-0.158204397677296,-0.018008517098262,
0.0412001204550104));
#21283=CARTESIAN_POINT('Ctrl Pts',(-0.103683798437843,0.120866071826586,
0.0334401445460125));
#21284=CARTESIAN_POINT('Ctrl Pts',(0.0419114400718942,0.153619241427338,
0.0256801686370146));
#21285=CARTESIAN_POINT('Ctrl Pts',(0.150617189657149,0.051532037718835,
0.0179201927280167));
#21286=CARTESIAN_POINT('Ctrl Pts',(0.127277973887939,-0.0958397618555833,
0.0101602168190187));
#21287=CARTESIAN_POINT('Ctrl Pts',(-0.00816462298486686,-0.1589878257446,
0.00240024091002091));
#21288=CARTESIAN_POINT('Ctrl Pts',(-0.0931288011773165,-0.108153310201063,
-0.00277307636264444));
#21289=CARTESIAN_POINT('Ctrl Pts',(-0.116025084863626,-0.0704394595391406,
-0.00535973499897709));
#21290=CARTESIAN_POINT('Ctrl Pts',(-0.0326585063531099,-0.122159831625555,
0.256079204996931));
#21291=CARTESIAN_POINT('Ctrl Pts',(-0.0723664509947957,-0.111544213176404,
0.253492546360598));
#21292=CARTESIAN_POINT('Ctrl Pts',(-0.140030416338279,-0.0488579767430688,
0.248319229087933));
#21293=CARTESIAN_POINT('Ctrl Pts',(-0.118967245221113,0.0887588307916541,
0.240559253178936));
#21294=CARTESIAN_POINT('Ctrl Pts',(0.00670985822758596,0.148149427811594,
0.232799277269937));
#21295=CARTESIAN_POINT('Ctrl Pts',(0.126408941446163,0.0776306004621497,
0.225039301360939));
#21296=CARTESIAN_POINT('Ctrl Pts',(0.13517819575905,-0.0611197284766509,
0.217279325451942));
#21297=CARTESIAN_POINT('Ctrl Pts',(0.0252495680894444,-0.146171195674918,
0.209519349542944));
#21298=CARTESIAN_POINT('Ctrl Pts',(-0.106833312629116,-0.102919543721916,
0.201759373633946));
#21299=CARTESIAN_POINT('Ctrl Pts',(-0.14513297882358,0.0306973783801131,
0.193999397724948));
#21300=CARTESIAN_POINT('Ctrl Pts',(-0.0560158138568844,0.137358846829434,
0.18623942181595));
#21301=CARTESIAN_POINT('Ctrl Pts',(0.0822762555999414,0.12343505531591,
0.178479445906952));
#21302=CARTESIAN_POINT('Ctrl Pts',(0.148338312079331,0.00114501560774606,
0.170719469997954));
#21303=CARTESIAN_POINT('Ctrl Pts',(0.0841725061462688,-0.122149375503312,
0.162959494088956));
#21304=CARTESIAN_POINT('Ctrl Pts',(-0.0538887351138648,-0.138208332524951,
0.155199518179959));
#21305=CARTESIAN_POINT('Ctrl Pts',(-0.144640776437932,-0.0329328768327946,
0.14743954227096));
#21306=CARTESIAN_POINT('Ctrl Pts',(-0.108411473928508,0.101254481475986,
0.139679566361963));
#21307=CARTESIAN_POINT('Ctrl Pts',(0.0229930583633497,0.146549809237466,
0.131919590452964));
#21308=CARTESIAN_POINT('Ctrl Pts',(0.134211845731212,0.0631878768899486,
0.124159614543967));
#21309=CARTESIAN_POINT('Ctrl Pts',(0.127604957650822,-0.0756471577870196,
0.116399638634969));
#21310=CARTESIAN_POINT('Ctrl Pts',(0.00897276139199077,-0.148070990197453,
0.108639662725971));
#21311=CARTESIAN_POINT('Ctrl Pts',(-0.117536835702253,-0.0905021060782641,
0.100879686816973));
#21312=CARTESIAN_POINT('Ctrl Pts',(-0.140859658455999,0.0465192148090667,
0.0931197109079749));
#21313=CARTESIAN_POINT('Ctrl Pts',(-0.0405211996564747,0.142701080127962,
0.0853597349989771));
#21314=CARTESIAN_POINT('Ctrl Pts',(0.0953921089266558,0.113604316251249,
0.077599759089979));
#21315=CARTESIAN_POINT('Ctrl Pts',(0.147558089427783,-0.0152261107569683,
0.0698397831809813));
#21316=CARTESIAN_POINT('Ctrl Pts',(0.070185198446632,-0.130690276993449,
0.0620798072719832));
#21317=CARTESIAN_POINT('Ctrl Pts',(-0.0688105409485176,-0.131418790976063,
0.0543198313629854));
#21318=CARTESIAN_POINT('Ctrl Pts',(-0.147384180400005,-0.0167768442073323,
0.0465598554539874));
#21319=CARTESIAN_POINT('Ctrl Pts',(-0.0965924580977301,0.112599568633142,
0.0387998795449896));
#21320=CARTESIAN_POINT('Ctrl Pts',(0.0390449528272914,0.143112620912232,
0.0310399036359916));
#21321=CARTESIAN_POINT('Ctrl Pts',(0.140315891199508,0.0480075601882123,
0.0232799277269937));
#21322=CARTESIAN_POINT('Ctrl Pts',(0.118572935644375,-0.0892849058445864,
0.0155199518179958));
#21323=CARTESIAN_POINT('Ctrl Pts',(-0.00760621249830358,-0.148114026758875,
0.00775997590899793));
#21324=CARTESIAN_POINT('Ctrl Pts',(-0.0867593583659504,-0.100756282477341,
0.00258665863633259));
#21325=CARTESIAN_POINT('Ctrl Pts',(-0.108089675695031,-0.0656218295092657,
-5.55111512312578E-17));
#21326=CARTESIAN_POINT('Ctrl Pts',(-0.108089675695031,-0.0656218295092657,
-5.55111512312578E-17));
#21327=CARTESIAN_POINT('Ctrl Pts',(-0.104219465379748,-0.0739058869203245,
-4.02841154597017E-17));
#21328=CARTESIAN_POINT('Ctrl Pts',(-0.0994141168358061,-0.0816768736924768,
-5.16144647363644E-17));
#21329=CARTESIAN_POINT('Ctrl Pts',(-0.0938412360364922,-0.088871564406415,
-3.81639164714898E-17));
#21330=CARTESIAN_POINT('Ctrl Pts',(-0.0894001862863345,-0.094605040600905,
-2.74451237748006E-17));
#21331=CARTESIAN_POINT('Ctrl Pts',(-0.0844703330957707,-0.0999727304469881,
3.12377098840079E-17));
#21332=CARTESIAN_POINT('Ctrl Pts',(-0.0791158513129458,-0.104935071387697,
-1.21430643318376E-17));
#21333=CARTESIAN_POINT('Ctrl Pts',(-0.0766900604813501,-0.107183206995485,
-3.17962611543325E-17));
#21334=CARTESIAN_POINT('Ctrl Pts',(-0.0741829996358932,-0.109342173006691,
4.83248416902999E-17));
#21335=CARTESIAN_POINT('Ctrl Pts',(-0.0716059924168524,-0.111405381598006,
5.3776427755281E-17));
#21336=CARTESIAN_POINT('Ctrl Pts',(-0.0639212992135713,-0.117557915794061,
7.00331794132204E-17));
#21337=CARTESIAN_POINT('Ctrl Pts',(-0.0556061968393146,-0.12287204611112,
-5.69073736333764E-18));
#21338=CARTESIAN_POINT('Ctrl Pts',(-0.0468203466856493,-0.127256781127915,
5.55111512312578E-17));
#21339=CARTESIAN_POINT('Ctrl Pts',(-0.0434613267337519,-0.12893315986732,
7.89099528597243E-17));
#21340=CARTESIAN_POINT('Ctrl Pts',(-0.0400330653128497,-0.130473352587733,
3.97002991909352E-17));
#21341=CARTESIAN_POINT('Ctrl Pts',(-0.0365431560942257,-0.131870761756357,
6.59194920871187E-17));
#21342=CARTESIAN_POINT('Ctrl Pts',(-0.0339571636773035,-0.13290622981212,
8.5347686277821E-17));
#21343=CARTESIAN_POINT('Ctrl Pts',(-0.0313383144727484,-0.133862652235137,
-2.74403076010104E-17));
#21344=CARTESIAN_POINT('Ctrl Pts',(-0.0286994266230122,-0.134734580282325,
-2.42861286636753E-17));
#21345=CARTESIAN_POINT('Ctrl Pts',(-0.0216199050576346,-0.137073760181214,
-1.58242011095522E-17));
#21346=CARTESIAN_POINT('Ctrl Pts',(-0.0143790427459088,-0.138813119073991,
5.80198461902811E-17));
#21347=CARTESIAN_POINT('Ctrl Pts',(-0.0070411538297537,-0.139912507657099,
6.93889390390723E-17));
#21348=CARTESIAN_POINT('Ctrl Pts',(5.47883476400097E-5,-0.140975646920361,
8.02325614020808E-17));
#21349=CARTESIAN_POINT('Ctrl Pts',(0.00724182591717642,-0.141440539972256,
1.32011341321413E-16));
#21350=CARTESIAN_POINT('Ctrl Pts',(0.0144605478337719,-0.141339082434075,
1.61329283265843E-16));
#21351=CARTESIAN_POINT('Ctrl Pts',(0.0178811722145177,-0.141291006315792,
1.75221724083914E-16));
#21352=CARTESIAN_POINT('Ctrl Pts',(0.021310106848269,-0.141115105569205,
1.85534911235541E-16));
#21353=CARTESIAN_POINT('Ctrl Pts',(0.0247235715439624,-0.140816220288761,
1.71737624121704E-16));
#21354=CARTESIAN_POINT('Ctrl Pts',(0.0339754553361668,-0.140006119078294,
1.34341339582434E-16));
#21355=CARTESIAN_POINT('Ctrl Pts',(0.0431421008898472,-0.138295657968001,
8.04496487960062E-17));
#21356=CARTESIAN_POINT('Ctrl Pts',(0.0520992976556894,-0.135759125106636,
3.20923843055709E-17));
#21357=CARTESIAN_POINT('Ctrl Pts',(0.0590658916121619,-0.13378629867842,
-5.518202506064E-18));
#21358=CARTESIAN_POINT('Ctrl Pts',(0.0659062642374416,-0.131312982137409,
7.87850579480063E-17));
#21359=CARTESIAN_POINT('Ctrl Pts',(0.0725619642951071,-0.128359965266718,
7.63278329429795E-17));
#21360=CARTESIAN_POINT('Ctrl Pts',(0.0758074813473741,-0.126919986522721,
7.51296170399226E-17));
#21361=CARTESIAN_POINT('Ctrl Pts',(0.0790005264283722,-0.125369490597537,
8.38688896655138E-17));
#21362=CARTESIAN_POINT('Ctrl Pts',(0.0821329715644795,-0.123712761836801,
7.24247051220317E-17));
#21363=CARTESIAN_POINT('Ctrl Pts',(0.0888257654942848,-0.120172989003949,
4.79730178566093E-17));
#21364=CARTESIAN_POINT('Ctrl Pts',(0.0952446087626691,-0.116147988031934,
8.96774285244103E-17));
#21365=CARTESIAN_POINT('Ctrl Pts',(0.101324221742587,-0.111663228753314,
8.28330459778925E-17));
#21366=CARTESIAN_POINT('Ctrl Pts',(0.104638321741973,-0.109218510516871,
7.91020571356516E-17));
#21367=CARTESIAN_POINT('Ctrl Pts',(0.107849695272814,-0.106637925639498,
3.17151869302413E-17));
#21368=CARTESIAN_POINT('Ctrl Pts',(0.110939265073957,-0.10393289123317,
1.53956708492942E-17));
#21369=CARTESIAN_POINT('Ctrl Pts',(0.115072333360666,-0.100314234708527,
-6.43574216607592E-18));
#21370=CARTESIAN_POINT('Ctrl Pts',(0.118992075260627,-0.0964697210975667,
5.54296751400654E-17));
#21371=CARTESIAN_POINT('Ctrl Pts',(0.122673447199167,-0.0924082746861152,
3.52365706057789E-17));
#21372=CARTESIAN_POINT('Ctrl Pts',(0.125092164655522,-0.0897398425098966,
2.31620156359627E-17));
#21373=CARTESIAN_POINT('Ctrl Pts',(0.127407959881093,-0.0869777021544565,
-4.01489640485901E-17));
#21374=CARTESIAN_POINT('Ctrl Pts',(0.129620323775263,-0.0841289546921697,
-3.98986399474666E-17));
#21375=CARTESIAN_POINT('Ctrl Pts',(-0.126471935391749,0.000101176582396995,
0.195658032638058));
#21376=CARTESIAN_POINT('Ctrl Pts',(-0.126547267107008,0.00888033934128026,
0.195105154333688));
#21377=CARTESIAN_POINT('Ctrl Pts',(-0.125707148272093,0.0176451944231377,
0.194552276029318));
#21378=CARTESIAN_POINT('Ctrl Pts',(-0.12389684029672,0.0262048027713284,
0.193999397724948));
#21379=CARTESIAN_POINT('Ctrl Pts',(-0.115427257168015,0.0662512011965534,
0.191412739088615));
#21380=CARTESIAN_POINT('Ctrl Pts',(-0.0857215355124495,0.101805024012994,
0.188826080452282));
#21381=CARTESIAN_POINT('Ctrl Pts',(-0.0478199964418627,0.117261303502293,
0.18623942181595));
#21382=CARTESIAN_POINT('Ctrl Pts',(-0.0099184573712758,0.132717582991593,
0.183652763179617));
#21383=CARTESIAN_POINT('Ctrl Pts',(0.0361788991143328,0.128076319153751,
0.181066104543285));
#21384=CARTESIAN_POINT('Ctrl Pts',(0.070237920103702,0.105374013950137,
0.178479445906952));
#21385=CARTESIAN_POINT('Ctrl Pts',(0.104296941093071,0.0826717087465222,
0.175892787270619));
#21386=CARTESIAN_POINT('Ctrl Pts',(0.126317626586201,0.0419083621771342,
0.173306128634287));
#21387=CARTESIAN_POINT('Ctrl Pts',(0.126633668343922,0.000977623707263797,
0.170719469997954));
#21388=CARTESIAN_POINT('Ctrl Pts',(0.126949710101644,-0.0399531147626067,
0.168132811361621));
#21389=CARTESIAN_POINT('Ctrl Pts',(0.105561108123956,-0.08105124513296,
0.165546152725289));
#21390=CARTESIAN_POINT('Ctrl Pts',(0.0718566002584231,-0.104276803155076,
0.162959494088956));
#21391=CARTESIAN_POINT('Ctrl Pts',(0.0381520923928904,-0.127502361177192,
0.160372835452623));
#21392=CARTESIAN_POINT('Ctrl Pts',(-0.00786832136048696,-0.132855346851071,
0.157786176816291));
#21393=CARTESIAN_POINT('Ctrl Pts',(-0.0460038684578537,-0.117985930405985,
0.155199518179958));
#21394=CARTESIAN_POINT('Ctrl Pts',(-0.0841394155552204,-0.103116513960899,
0.152612859543626));
#21395=CARTESIAN_POINT('Ctrl Pts',(-0.114390095996576,-0.0680246953968468,
0.150026200907293));
#21396=CARTESIAN_POINT('Ctrl Pts',(-0.12347721913235,-0.0281142263966907,
0.14743954227096));
#21397=CARTESIAN_POINT('Ctrl Pts',(-0.125563410841138,-0.018951712774069,
0.14684570572666));
#21398=CARTESIAN_POINT('Ctrl Pts',(-0.126534167537385,-0.00953522996602069,
0.146251869182359));
#21399=CARTESIAN_POINT('Ctrl Pts',(-0.126453631260982,-0.000102348163238207,
0.145658032638058));
#21400=CARTESIAN_POINT('Ctrl Pts',(-0.0398513841857245,-0.149064942821851,
0.24));
#21401=CARTESIAN_POINT('Ctrl Pts',(-0.0498806325786677,-0.145400296738327,
0.24));
#21402=CARTESIAN_POINT('Ctrl Pts',(-0.0594363948008725,-0.140639648297949,
0.24));
#21403=CARTESIAN_POINT('Ctrl Pts',(-0.0684062055177017,-0.134931499399492,
0.24));
#21404=CARTESIAN_POINT('Ctrl Pts',(-0.0735915624001909,-0.131631676235849,
0.24));
#21405=CARTESIAN_POINT('Ctrl Pts',(-0.0785806353345173,-0.128014298080738,
0.24));
#21406=CARTESIAN_POINT('Ctrl Pts',(-0.0833462611484583,-0.124102693747304,
0.24));
#21407=CARTESIAN_POINT('Ctrl Pts',(-0.0858656342542594,-0.122034803580736,
0.24));
#21408=CARTESIAN_POINT('Ctrl Pts',(-0.0883241156266364,-0.11988309220465,
0.24));
#21409=CARTESIAN_POINT('Ctrl Pts',(-0.0907117892851122,-0.117655751751618,
0.24));
#21410=CARTESIAN_POINT('Ctrl Pts',(-0.0983819858496404,-0.110500611839494,
0.24));
#21411=CARTESIAN_POINT('Ctrl Pts',(-0.105284458416918,-0.102606966330569,
0.24));
#21412=CARTESIAN_POINT('Ctrl Pts',(-0.111294422020379,-0.0941015332659665,
0.24));
#21413=CARTESIAN_POINT('Ctrl Pts',(-0.114410577497229,-0.0896914812962706,
0.24));
#21414=CARTESIAN_POINT('Ctrl Pts',(-0.117286101138547,-0.0851164738413172,
0.24));
#21415=CARTESIAN_POINT('Ctrl Pts',(-0.119898298320422,-0.0803922539627851,
0.24));
#21416=CARTESIAN_POINT('Ctrl Pts',(-0.1222721977331,-0.0760990011896685,
0.24));
#21417=CARTESIAN_POINT('Ctrl Pts',(-0.124430744329062,-0.0716759619599862,
0.24));
#21418=CARTESIAN_POINT('Ctrl Pts',(-0.126341093034125,-0.0671690272221462,
0.24));
#21419=CARTESIAN_POINT('Ctrl Pts',(-0.129206708925078,-0.060408406100978,
0.24));
#21420=CARTESIAN_POINT('Ctrl Pts',(-0.131522065955468,-0.0534490321795157,
0.24));
#21421=CARTESIAN_POINT('Ctrl Pts',(-0.133233091500091,-0.0463330844490581,
0.24));
#21422=CARTESIAN_POINT('Ctrl Pts',(-0.135004134506116,-0.0389675313754268,
0.24));
#21423=CARTESIAN_POINT('Ctrl Pts',(-0.136127599829873,-0.0314337185245799,
0.24));
#21424=CARTESIAN_POINT('Ctrl Pts',(-0.136615064298196,-0.0238138180582873,
0.24));
#21425=CARTESIAN_POINT('Ctrl Pts',(-0.136813484749433,-0.0207121682209076,
0.24));
#21426=CARTESIAN_POINT('Ctrl Pts',(-0.136906013213758,-0.0175970392000076,
0.24));
#21427=CARTESIAN_POINT('Ctrl Pts',(-0.136893785357156,-0.0144871321155608,
0.24));
#21428=CARTESIAN_POINT('Ctrl Pts',(-0.136861203984761,-0.00620072149302863,
0.24));
#21429=CARTESIAN_POINT('Ctrl Pts',(-0.136088646936857,0.00207357465703332,
0.24));
#21430=CARTESIAN_POINT('Ctrl Pts',(-0.134599584032292,0.0102285531249486,
0.24));
#21431=CARTESIAN_POINT('Ctrl Pts',(-0.133676409755049,0.0152843948425598,
0.24));
#21432=CARTESIAN_POINT('Ctrl Pts',(-0.132477333465274,0.0202942984003417,
0.24));
#21433=CARTESIAN_POINT('Ctrl Pts',(-0.131003622030167,0.0252303138624672,
0.24));
#21434=CARTESIAN_POINT('Ctrl Pts',(-0.129740734874544,0.029460199292259,
0.24));
#21435=CARTESIAN_POINT('Ctrl Pts',(-0.128274507607502,0.0336384499732856,
0.24));
#21436=CARTESIAN_POINT('Ctrl Pts',(-0.126614574688298,0.0377237273426867,
0.24));
#21437=CARTESIAN_POINT('Ctrl Pts',(-0.124573382985647,0.042747324485064,
0.24));
#21438=CARTESIAN_POINT('Ctrl Pts',(-0.122237651925267,0.0476379767326878,
0.24));
#21439=CARTESIAN_POINT('Ctrl Pts',(-0.119609691052418,0.0523617558795304,
0.24));
#21440=CARTESIAN_POINT('Ctrl Pts',(-0.117006563775536,0.0570408964535612,
0.24));
#21441=CARTESIAN_POINT('Ctrl Pts',(-0.114113358229268,0.0615597689541448,
0.24));
#21442=CARTESIAN_POINT('Ctrl Pts',(-0.110947628485839,0.0658586917144141,
0.24));
#21443=CARTESIAN_POINT('Ctrl Pts',(-0.108265305855902,0.0695011687224882,
0.24));
#21444=CARTESIAN_POINT('Ctrl Pts',(-0.105385772272888,0.0729892759232728,
0.24));
#21445=CARTESIAN_POINT('Ctrl Pts',(-0.102309360287629,0.0763011815833395,
0.24));
#21446=CARTESIAN_POINT('Ctrl Pts',(-0.100282916666232,0.0784827457339379,
0.24));
#21447=CARTESIAN_POINT('Ctrl Pts',(-0.0981709975111385,0.0805877996091198,
0.24));
#21448=CARTESIAN_POINT('Ctrl Pts',(-0.0959791030802606,0.0826138105732947,
0.24));
#21449=CARTESIAN_POINT('Origin',(0.,0.,0.24));
#21450=CARTESIAN_POINT('',(0.158771324027147,-0.275,0.24));
#21451=CARTESIAN_POINT('',(0.317542648054294,0.,0.24));
#21452=CARTESIAN_POINT('',(0.158771324027147,-0.275,0.24));
#21453=CARTESIAN_POINT('',(0.158771324027147,0.275,0.24));
#21454=CARTESIAN_POINT('',(0.317542648054294,0.,0.24));
#21455=CARTESIAN_POINT('',(-0.158771324027147,0.275,0.24));
#21456=CARTESIAN_POINT('',(0.158771324027147,0.275,0.24));
#21457=CARTESIAN_POINT('',(-0.317542648054294,5.55111512312578E-17,0.24));
#21458=CARTESIAN_POINT('',(-0.158771324027147,0.275,0.24));
#21459=CARTESIAN_POINT('',(-0.158771324027147,-0.275,0.24));
#21460=CARTESIAN_POINT('',(-0.317542648054294,3.88877587532466E-17,0.24));
#21461=CARTESIAN_POINT('',(-0.158771324027147,-0.275,0.24));
#21462=CARTESIAN_POINT('Origin',(0.,0.,0.12));
#21463=CARTESIAN_POINT('Origin',(-0.158771324027147,-0.275,0.));
#21464=CARTESIAN_POINT('',(-0.158771324027147,-0.275,0.));
#21465=CARTESIAN_POINT('',(0.158771324027147,-0.275,0.));
#21466=CARTESIAN_POINT('',(-0.158771324027147,-0.275,0.));
#21467=CARTESIAN_POINT('',(0.158771324027147,-0.275,0.));
#21468=CARTESIAN_POINT('',(-0.158771324027147,-0.275,0.));
#21469=CARTESIAN_POINT('Origin',(-0.317542648054294,3.88877587532466E-17,
0.));
#21470=CARTESIAN_POINT('',(-0.317542648054294,3.88877587532466E-17,0.));
#21471=CARTESIAN_POINT('',(-0.317542648054294,3.88877587532466E-17,0.));
#21472=CARTESIAN_POINT('',(-0.317542648054294,3.88877587532466E-17,0.));
#21473=CARTESIAN_POINT('Origin',(-0.158771324027147,0.275,0.));
#21474=CARTESIAN_POINT('',(-0.158771324027147,0.275,0.));
#21475=CARTESIAN_POINT('',(-0.158771324027147,0.275,0.));
#21476=CARTESIAN_POINT('',(-0.158771324027147,0.275,0.));
#21477=CARTESIAN_POINT('Origin',(0.158771324027147,0.275,0.));
#21478=CARTESIAN_POINT('',(0.158771324027147,0.275,0.));
#21479=CARTESIAN_POINT('',(0.158771324027147,0.275,0.));
#21480=CARTESIAN_POINT('',(0.158771324027147,0.275,0.));
#21481=CARTESIAN_POINT('Origin',(0.317542648054294,0.,0.));
#21482=CARTESIAN_POINT('',(0.317542648054294,0.,0.));
#21483=CARTESIAN_POINT('',(0.317542648054294,0.,0.));
#21484=CARTESIAN_POINT('',(0.317542648054294,0.,0.));
#21485=CARTESIAN_POINT('Origin',(0.158771324027147,-0.275,0.));
#21486=CARTESIAN_POINT('',(0.158771324027147,-0.275,0.));
#21487=CARTESIAN_POINT('Origin',(0.,0.,0.));
#21488=CARTESIAN_POINT('',(0.,0.,0.));
#21489=CARTESIAN_POINT('Origin',(2.,0.,1.));
#21490=CARTESIAN_POINT('',(1.65,4.28626379701574E-17,1.1));
#21491=CARTESIAN_POINT('Origin',(2.,0.,1.1));
#21492=CARTESIAN_POINT('',(1.65,4.28626379701574E-17,0.9));
#21493=CARTESIAN_POINT('',(1.65,4.28626379701574E-17,1.));
#21494=CARTESIAN_POINT('Origin',(2.,0.,0.9));
#21495=CARTESIAN_POINT('Origin',(8.8,0.,1.));
#21496=CARTESIAN_POINT('',(8.45,4.28626379701574E-17,1.1));
#21497=CARTESIAN_POINT('Origin',(8.8,0.,1.1));
#21498=CARTESIAN_POINT('',(8.45,4.28626379701574E-17,0.9));
#21499=CARTESIAN_POINT('',(8.45,4.28626379701574E-17,1.));
#21500=CARTESIAN_POINT('Origin',(8.8,0.,0.9));
#21501=CARTESIAN_POINT('Origin',(8.1,1.,0.7));
#21502=CARTESIAN_POINT('',(7.85,1.,0.7));
#21503=CARTESIAN_POINT('Origin',(8.1,1.,0.7));
#21504=CARTESIAN_POINT('',(7.95,1.,0.7));
#21505=CARTESIAN_POINT('Origin',(8.1,1.,0.7));
#21506=CARTESIAN_POINT('Origin',(8.1,1.,0.7));
#21507=CARTESIAN_POINT('',(7.85,1.,0.6));
#21508=CARTESIAN_POINT('Origin',(8.1,1.,0.6));
#21509=CARTESIAN_POINT('',(7.85,1.,0.7));
#21510=CARTESIAN_POINT('Origin',(8.1,1.,0.6));
#21511=CARTESIAN_POINT('Origin',(2.7,-1.,0.7));
#21512=CARTESIAN_POINT('',(2.45,-1.,0.7));
#21513=CARTESIAN_POINT('Origin',(2.7,-1.,0.7));
#21514=CARTESIAN_POINT('',(2.55,-1.,0.7));
#21515=CARTESIAN_POINT('Origin',(2.7,-1.,0.7));
#21516=CARTESIAN_POINT('Origin',(2.7,-1.,0.7));
#21517=CARTESIAN_POINT('',(2.45,-1.,0.6));
#21518=CARTESIAN_POINT('Origin',(2.7,-1.,0.6));
#21519=CARTESIAN_POINT('',(2.45,-1.,0.7));
#21520=CARTESIAN_POINT('Origin',(2.7,-1.,0.6));
#21521=CARTESIAN_POINT('Origin',(2.7,1.,0.7));
#21522=CARTESIAN_POINT('',(2.45,1.,0.7));
#21523=CARTESIAN_POINT('Origin',(2.7,1.,0.7));
#21524=CARTESIAN_POINT('',(2.55,1.,0.7));
#21525=CARTESIAN_POINT('Origin',(2.7,1.,0.7));
#21526=CARTESIAN_POINT('Origin',(2.7,1.,0.7));
#21527=CARTESIAN_POINT('',(2.45,1.,0.6));
#21528=CARTESIAN_POINT('Origin',(2.7,1.,0.6));
#21529=CARTESIAN_POINT('',(2.45,1.,0.7));
#21530=CARTESIAN_POINT('Origin',(2.7,1.,0.6));
#21531=CARTESIAN_POINT('Origin',(8.1,-1.,0.7));
#21532=CARTESIAN_POINT('',(7.85,-1.,0.7));
#21533=CARTESIAN_POINT('Origin',(8.1,-1.,0.7));
#21534=CARTESIAN_POINT('',(7.95,-1.,0.7));
#21535=CARTESIAN_POINT('Origin',(8.1,-1.,0.7));
#21536=CARTESIAN_POINT('Origin',(8.1,-1.,0.7));
#21537=CARTESIAN_POINT('',(7.85,-1.,0.6));
#21538=CARTESIAN_POINT('Origin',(8.1,-1.,0.6));
#21539=CARTESIAN_POINT('',(7.85,-1.,0.7));
#21540=CARTESIAN_POINT('Origin',(8.1,-1.,0.6));
#21541=CARTESIAN_POINT('Origin',(8.1,1.,0.9));
#21542=CARTESIAN_POINT('',(7.95,1.,0.9));
#21543=CARTESIAN_POINT('',(7.95,1.,0.9));
#21544=CARTESIAN_POINT('Origin',(8.1,1.,0.9));
#21545=CARTESIAN_POINT('Origin',(2.7,-1.,0.9));
#21546=CARTESIAN_POINT('',(2.55,-1.,0.9));
#21547=CARTESIAN_POINT('',(2.55,-1.,0.9));
#21548=CARTESIAN_POINT('Origin',(2.7,-1.,0.9));
#21549=CARTESIAN_POINT('Origin',(2.7,1.,0.9));
#21550=CARTESIAN_POINT('',(2.55,1.,0.9));
#21551=CARTESIAN_POINT('',(2.55,1.,0.9));
#21552=CARTESIAN_POINT('Origin',(2.7,1.,0.9));
#21553=CARTESIAN_POINT('Origin',(8.1,-1.,0.9));
#21554=CARTESIAN_POINT('',(7.95,-1.,0.9));
#21555=CARTESIAN_POINT('',(7.95,-1.,0.9));
#21556=CARTESIAN_POINT('Origin',(8.1,-1.,0.9));
#21557=CARTESIAN_POINT('Ctrl Pts',(10.3006295894369,0.974894988741159,1.1));
#21558=CARTESIAN_POINT('Ctrl Pts',(10.315705472156,0.974011521809381,1.1));
#21559=CARTESIAN_POINT('Ctrl Pts',(10.3502474882039,0.960160784532573,1.1));
#21560=CARTESIAN_POINT('Ctrl Pts',(10.3664342774515,0.92524659453289,1.1));
#21561=CARTESIAN_POINT('Ctrl Pts',(10.3664342774515,0.905110932257975,1.1));
#21562=CARTESIAN_POINT('Ctrl Pts',(10.3019806204244,0.997949597787003,1.1));
#21563=CARTESIAN_POINT('Ctrl Pts',(10.3220349090938,0.996609784625678,1.09999398337427));
#21564=CARTESIAN_POINT('Ctrl Pts',(10.3677183242066,0.978025516808524,1.09998506712737));
#21565=CARTESIAN_POINT('Ctrl Pts',(10.3893396302527,0.931918448901421,1.09999143472557));
#21566=CARTESIAN_POINT('Ctrl Pts',(10.3895723566779,0.905110932257975,1.1));
#21567=CARTESIAN_POINT('Ctrl Pts',(10.3043223099121,1.03790925537118,1.08136572286424));
#21568=CARTESIAN_POINT('Ctrl Pts',(10.3329503749445,1.0358015962555,1.08164234815929));
#21569=CARTESIAN_POINT('Ctrl Pts',(10.3979372989902,1.00899285190124,1.08203919297574));
#21570=CARTESIAN_POINT('Ctrl Pts',(10.4290660105163,0.943405843911333,1.08168333012239));
#21571=CARTESIAN_POINT('Ctrl Pts',(10.4296737498558,0.905110932257975,1.08129070628762));
#21572=CARTESIAN_POINT('Ctrl Pts',(10.3052465815697,1.05368144854439,1.04171131144128));
#21573=CARTESIAN_POINT('Ctrl Pts',(10.3373036016374,1.05157771141627,1.04242733672965));
#21574=CARTESIAN_POINT('Ctrl Pts',(10.4104769365187,1.02185126978705,1.04346621563788));
#21575=CARTESIAN_POINT('Ctrl Pts',(10.445100550936,0.94795146444073,1.04253150017828));
#21576=CARTESIAN_POINT('Ctrl Pts',(10.4454164251054,0.905110932257975,1.0415166534692));
#21577=CARTESIAN_POINT('Ctrl Pts',(10.3053025283406,1.05463614976313,1.02441711227736));
#21578=CARTESIAN_POINT('Ctrl Pts',(10.3375636805833,1.05269876817044,1.02526261130878));
#21579=CARTESIAN_POINT('Ctrl Pts',(10.411517621087,1.0229540574362,1.02649649899074));
#21580=CARTESIAN_POINT('Ctrl Pts',(10.4462618831994,0.948196125723061,1.02538435201347));
#21581=CARTESIAN_POINT('Ctrl Pts',(10.4463246402318,0.905110932257975,1.02418687649944));
#21582=CARTESIAN_POINT('',(10.3664342774515,0.905110932257975,1.1));
#21583=CARTESIAN_POINT('',(10.4463246402318,0.905110932257975,1.02418687649943));
#21584=CARTESIAN_POINT('Origin',(10.3664342774515,0.905110932257975,1.02));
#21585=CARTESIAN_POINT('',(10.3053025283406,1.05463614976313,1.02441711227738));
#21586=CARTESIAN_POINT('Ctrl Pts',(10.4463246402318,0.905110932257975,1.02418687649944));
#21587=CARTESIAN_POINT('Ctrl Pts',(10.4462618831994,0.948196125723061,1.02538435201347));
#21588=CARTESIAN_POINT('Ctrl Pts',(10.411517621087,1.0229540574362,1.02649649899074));
#21589=CARTESIAN_POINT('Ctrl Pts',(10.3375636805833,1.05269876817044,1.02526261130878));
#21590=CARTESIAN_POINT('Ctrl Pts',(10.3053025283406,1.05463614976313,1.02441711227736));
#21591=CARTESIAN_POINT('',(10.3006295894369,0.974894988741159,1.1));
#21592=CARTESIAN_POINT('Origin',(10.3006295894369,0.974894988741159,1.02));
#21593=CARTESIAN_POINT('Ctrl Pts',(10.3006295894369,0.974894988741159,1.1));
#21594=CARTESIAN_POINT('Ctrl Pts',(10.315705472156,0.974011521809381,1.1));
#21595=CARTESIAN_POINT('Ctrl Pts',(10.3502474882039,0.960160784532573,1.1));
#21596=CARTESIAN_POINT('Ctrl Pts',(10.3664342774515,0.92524659453289,1.1));
#21597=CARTESIAN_POINT('Ctrl Pts',(10.3664342774515,0.905110932257975,1.1));
#21598=CARTESIAN_POINT('Origin',(10.3664342774515,0.526416499322631,1.02));
#21599=CARTESIAN_POINT('',(10.3664342774515,-0.905110932257974,1.1));
#21600=CARTESIAN_POINT('',(10.4463246402318,-0.905110932257974,1.02418687649944));
#21601=CARTESIAN_POINT('Origin',(10.3664342774515,-0.905110932257974,1.02));
#21602=CARTESIAN_POINT('',(10.4463246402318,0.526416499322631,1.02418687649944));
#21603=CARTESIAN_POINT('',(10.3664342774515,0.526416499322631,1.1));
#21604=CARTESIAN_POINT('Ctrl Pts',(10.3664342774515,-0.905110932257974,
1.1));
#21605=CARTESIAN_POINT('Ctrl Pts',(10.3664342774515,-0.920212678972614,
1.1));
#21606=CARTESIAN_POINT('Ctrl Pts',(10.3546350195413,-0.955507038097987,
1.1));
#21607=CARTESIAN_POINT('Ctrl Pts',(10.3207307664069,-0.973717032831462,
1.1));
#21608=CARTESIAN_POINT('Ctrl Pts',(10.3006295894369,-0.974894988741159,
1.1));
#21609=CARTESIAN_POINT('Ctrl Pts',(10.3895723566779,-0.905110932257974,
1.1));
#21610=CARTESIAN_POINT('Ctrl Pts',(10.3893978118589,-0.925216569751813,
1.09999357604418));
#21611=CARTESIAN_POINT('Ctrl Pts',(10.3734893817427,-0.971910228734235,
1.09998467394719));
#21612=CARTESIAN_POINT('Ctrl Pts',(10.3287196719985,-0.996163180237569,
1.09999197783236));
#21613=CARTESIAN_POINT('Ctrl Pts',(10.3019806204244,-0.997949597787003,
1.1));
#21614=CARTESIAN_POINT('Ctrl Pts',(10.4296737498558,-0.905110932257974,
1.0812907062876));
#21615=CARTESIAN_POINT('Ctrl Pts',(10.4292179453509,-0.933832116014069,
1.08158517416384));
#21616=CARTESIAN_POINT('Ctrl Pts',(10.4061705706524,-1.00027633256302,1.08203447943735));
#21617=CARTESIAN_POINT('Ctrl Pts',(10.3424930633099,-1.03509904321534,1.08173455659116));
#21618=CARTESIAN_POINT('Ctrl Pts',(10.3043223099121,-1.03790925537115,1.08136572286421));
#21619=CARTESIAN_POINT('Ctrl Pts',(10.4454164251054,-0.905110932257974,
1.0415166534692));
#21620=CARTESIAN_POINT('Ctrl Pts',(10.4451795194782,-0.937241331413026,
1.04227778850144));
#21621=CARTESIAN_POINT('Ctrl Pts',(10.4197512278104,-1.01202259423409,1.0434534732467));
#21622=CARTESIAN_POINT('Ctrl Pts',(10.3479892750172,-1.05087646570533,1.0426660118263));
#21623=CARTESIAN_POINT('Ctrl Pts',(10.3052465815697,-1.05368144854438,1.04171131144128));
#21624=CARTESIAN_POINT('Ctrl Pts',(10.4463246402318,-0.905110932257974,
1.02418687649944));
#21625=CARTESIAN_POINT('Ctrl Pts',(10.4462775724575,-0.937424827374877,
1.02508498313546));
#21626=CARTESIAN_POINT('Ctrl Pts',(10.4209202812412,-1.01298254961426,1.02648109501254));
#21627=CARTESIAN_POINT('Ctrl Pts',(10.3483173980216,-1.05205297430477,1.02554444431988));
#21628=CARTESIAN_POINT('Ctrl Pts',(10.3053025283406,-1.05463614976313,1.02441711227736));
#21629=CARTESIAN_POINT('',(10.3006295894369,-0.974894988741159,1.1));
#21630=CARTESIAN_POINT('',(10.3053025283406,-1.05463614976313,1.02441711227736));
#21631=CARTESIAN_POINT('Origin',(10.3006295894369,-0.974894988741159,1.02));
#21632=CARTESIAN_POINT('Ctrl Pts',(10.3053025283406,-1.05463614976313,1.02441711227736));
#21633=CARTESIAN_POINT('Ctrl Pts',(10.3483173980216,-1.05205297430477,1.02554444431988));
#21634=CARTESIAN_POINT('Ctrl Pts',(10.4209202812412,-1.01298254961426,1.02648109501254));
#21635=CARTESIAN_POINT('Ctrl Pts',(10.4462775724575,-0.937424827374877,
1.02508498313546));
#21636=CARTESIAN_POINT('Ctrl Pts',(10.4463246402318,-0.905110932257974,
1.02418687649944));
#21637=CARTESIAN_POINT('Ctrl Pts',(10.3664342774515,-0.905110932257974,
1.1));
#21638=CARTESIAN_POINT('Ctrl Pts',(10.3664342774515,-0.920212678972614,
1.1));
#21639=CARTESIAN_POINT('Ctrl Pts',(10.3546350195413,-0.955507038097987,
1.1));
#21640=CARTESIAN_POINT('Ctrl Pts',(10.3207307664069,-0.973717032831462,
1.1));
#21641=CARTESIAN_POINT('Ctrl Pts',(10.3006295894369,-0.974894988741159,
1.1));
#21642=CARTESIAN_POINT('Ctrl Pts',(10.3006295894369,-0.974894988741159,
1.1));
#21643=CARTESIAN_POINT('Ctrl Pts',(8.90133038997308,-1.05689579714676,1.1));
#21644=CARTESIAN_POINT('Ctrl Pts',(5.63386529032775,-1.20659234980357,1.1));
#21645=CARTESIAN_POINT('Ctrl Pts',(2.35953432096223,-1.1387902266302,1.1));
#21646=CARTESIAN_POINT('Ctrl Pts',(0.497468741075922,-0.978719373910683,
1.1));
#21647=CARTESIAN_POINT('Ctrl Pts',(10.3019806204244,-0.997949597787003,
1.1));
#21648=CARTESIAN_POINT('Ctrl Pts',(8.90248440956766,-1.07998148241326,1.10000071389857));
#21649=CARTESIAN_POINT('Ctrl Pts',(5.63428345559727,-1.22975661509925,1.09999860206726));
#21650=CARTESIAN_POINT('Ctrl Pts',(2.35854977485598,-1.16192218645588,1.10000206853834));
#21651=CARTESIAN_POINT('Ctrl Pts',(0.495492436783665,-1.00170924455528,
1.1));
#21652=CARTESIAN_POINT('Ctrl Pts',(10.3043223112023,-1.03790927738781,1.08136574244164));
#21653=CARTESIAN_POINT('Ctrl Pts',(8.90448672538924,-1.11999254202045,1.08133291965814));
#21654=CARTESIAN_POINT('Ctrl Pts',(5.63501252140964,-1.26990499402305,1.08126385742935));
#21655=CARTESIAN_POINT('Ctrl Pts',(2.35683262246169,-1.20200947624765,1.08130376582018));
#21656=CARTESIAN_POINT('Ctrl Pts',(0.492066872450609,-1.0415580073244,1.08139899772624));
#21657=CARTESIAN_POINT('Ctrl Pts',(10.3052465815697,-1.05368144854439,1.04171131144128));
#21658=CARTESIAN_POINT('Ctrl Pts',(8.90527383415966,-1.13574844311122,1.04162635195479));
#21659=CARTESIAN_POINT('Ctrl Pts',(5.63529344743191,-1.28563363803111,1.04144655753461));
#21660=CARTESIAN_POINT('Ctrl Pts',(2.35616768559357,-1.21776439538312,1.04155103737704));
#21661=CARTESIAN_POINT('Ctrl Pts',(0.490711556403977,-1.05732407164794,
1.04179769276967));
#21662=CARTESIAN_POINT('Ctrl Pts',(10.3053025283406,-1.05463614976313,1.02441711227736));
#21663=CARTESIAN_POINT('Ctrl Pts',(8.90532084970199,-1.13668250951809,1.02431679017323));
#21664=CARTESIAN_POINT('Ctrl Pts',(5.63530902077156,-1.28652517622799,1.02410366945797));
#21665=CARTESIAN_POINT('Ctrl Pts',(2.35612886002319,-1.2186808487933,1.02422798328229));
#21666=CARTESIAN_POINT('Ctrl Pts',(0.490627822843887,-1.05829812393464,
1.02451933428366));
#21667=CARTESIAN_POINT('',(0.497468741075922,-0.978719373910683,1.1));
#21668=CARTESIAN_POINT('',(0.490627822843887,-1.05829812393464,1.02451933428366));
#21669=CARTESIAN_POINT('Origin',(0.497468741075922,-0.978719373910683,1.02));
#21670=CARTESIAN_POINT('Ctrl Pts',(0.490627822843887,-1.05829812393464,
1.02451933428366));
#21671=CARTESIAN_POINT('Ctrl Pts',(2.35612886002319,-1.2186808487933,1.02422798328229));
#21672=CARTESIAN_POINT('Ctrl Pts',(5.63530902077156,-1.28652517622799,1.02410366945797));
#21673=CARTESIAN_POINT('Ctrl Pts',(8.90532084970199,-1.13668250951809,1.02431679017323));
#21674=CARTESIAN_POINT('Ctrl Pts',(10.3053025283406,-1.05463614976313,1.02441711227736));
#21675=CARTESIAN_POINT('Ctrl Pts',(10.3006295894369,-0.974894988741159,
1.1));
#21676=CARTESIAN_POINT('Ctrl Pts',(8.90133038997308,-1.05689579714676,1.1));
#21677=CARTESIAN_POINT('Ctrl Pts',(5.63386529032775,-1.20659234980357,1.1));
#21678=CARTESIAN_POINT('Ctrl Pts',(2.35953432096223,-1.1387902266302,1.1));
#21679=CARTESIAN_POINT('Ctrl Pts',(0.497468741075922,-0.978719373910683,
1.1));
#21680=CARTESIAN_POINT('Ctrl Pts',(0.497468741075921,-0.978719373910683,
1.1));
#21681=CARTESIAN_POINT('Ctrl Pts',(0.482693827936028,-0.977449261315989,
1.1));
#21682=CARTESIAN_POINT('Ctrl Pts',(0.449140492346353,-0.963153189418853,
1.1));
#21683=CARTESIAN_POINT('Ctrl Pts',(0.433565722548535,-0.928845297374623,
1.1));
#21684=CARTESIAN_POINT('Ctrl Pts',(0.433565722548535,-0.909072757750428,
1.1));
#21685=CARTESIAN_POINT('Ctrl Pts',(0.495492436783665,-1.00170924455528,
1.1));
#21686=CARTESIAN_POINT('Ctrl Pts',(0.475845599502289,-0.99986336234735,
1.09999428725696));
#21687=CARTESIAN_POINT('Ctrl Pts',(0.431470670910625,-0.980707626108276,
1.09998595101222));
#21688=CARTESIAN_POINT('Ctrl Pts',(0.410656014536328,-0.935396857641307,
1.09999159501496));
#21689=CARTESIAN_POINT('Ctrl Pts',(0.410427643322096,-0.909072757750428,
1.1));
#21690=CARTESIAN_POINT('Ctrl Pts',(0.492065445269591,-1.04157460937658,
1.08141381101793));
#21691=CARTESIAN_POINT('Ctrl Pts',(0.464027324938814,-1.03875422423143,
1.08167681576789));
#21692=CARTESIAN_POINT('Ctrl Pts',(0.400896096452139,-1.01114975683443,
1.0820463630617));
#21693=CARTESIAN_POINT('Ctrl Pts',(0.370905720538455,-0.946677133941945,
1.08169093175476));
#21694=CARTESIAN_POINT('Ctrl Pts',(0.370309354350991,-0.909072757750428,
1.08130565542949));
#21695=CARTESIAN_POINT('Ctrl Pts',(0.490711556403977,-1.05732407164794,
1.04179769276967));
#21696=CARTESIAN_POINT('Ctrl Pts',(0.459302109313527,-1.05440855600651,
1.04247888820671));
#21697=CARTESIAN_POINT('Ctrl Pts',(0.388222412631638,-1.02376232464153,
1.04344633806995));
#21698=CARTESIAN_POINT('Ctrl Pts',(0.354893537837358,-0.951140796546497,
1.04251250847383));
#21699=CARTESIAN_POINT('Ctrl Pts',(0.354583574894625,-0.909072757750428,
1.0415166534692));
#21700=CARTESIAN_POINT('Ctrl Pts',(0.490627822843887,-1.05829812393464,
1.02451933428366));
#21701=CARTESIAN_POINT('Ctrl Pts',(0.459009463695281,-1.05553438344805,
1.02532396689517));
#21702=CARTESIAN_POINT('Ctrl Pts',(0.387169680965019,-1.0248398620393,1.02647307310763));
#21703=CARTESIAN_POINT('Ctrl Pts',(0.353736942373964,-0.951381046565094,
1.02536194261819));
#21704=CARTESIAN_POINT('Ctrl Pts',(0.35367535976817,-0.909072757750428,
1.02418687649944));
#21705=CARTESIAN_POINT('',(0.433565722548535,-0.909072757750428,1.1));
#21706=CARTESIAN_POINT('',(0.35367535976817,-0.909072757750428,1.02418687649944));
#21707=CARTESIAN_POINT('Origin',(0.433565722548536,-0.909072757750428,1.02));
#21708=CARTESIAN_POINT('Ctrl Pts',(0.35367535976817,-0.909072757750428,
1.02418687649944));
#21709=CARTESIAN_POINT('Ctrl Pts',(0.353736942373964,-0.951381046565094,
1.02536194261819));
#21710=CARTESIAN_POINT('Ctrl Pts',(0.387169680965019,-1.0248398620393,1.02647307310763));
#21711=CARTESIAN_POINT('Ctrl Pts',(0.459009463695281,-1.05553438344805,
1.02532396689517));
#21712=CARTESIAN_POINT('Ctrl Pts',(0.490627822843887,-1.05829812393464,
1.02451933428366));
#21713=CARTESIAN_POINT('Ctrl Pts',(0.497468741075921,-0.978719373910683,
1.1));
#21714=CARTESIAN_POINT('Ctrl Pts',(0.482693827936028,-0.977449261315989,
1.1));
#21715=CARTESIAN_POINT('Ctrl Pts',(0.449140492346353,-0.963153189418853,
1.1));
#21716=CARTESIAN_POINT('Ctrl Pts',(0.433565722548535,-0.928845297374623,
1.1));
#21717=CARTESIAN_POINT('Ctrl Pts',(0.433565722548535,-0.909072757750428,
1.1));
#21718=CARTESIAN_POINT('Origin',(0.433565722548535,-0.526416499322631,1.02));
#21719=CARTESIAN_POINT('',(0.433565722548535,0.909072757750428,1.1));
#21720=CARTESIAN_POINT('',(0.35367535976817,0.909072757750428,1.02418687649944));
#21721=CARTESIAN_POINT('Origin',(0.433565722548535,0.909072757750428,1.02));
#21722=CARTESIAN_POINT('',(0.35367535976817,-0.526416499322631,1.02418687649944));
#21723=CARTESIAN_POINT('',(0.433565722548535,-0.526416499322631,1.1));
#21724=CARTESIAN_POINT('Ctrl Pts',(0.433565722548535,0.909072757750428,
1.1));
#21725=CARTESIAN_POINT('Ctrl Pts',(0.433565722548535,0.923902162481473,
1.1));
#21726=CARTESIAN_POINT('Ctrl Pts',(0.444925688709976,0.95855828847753,1.1));
#21727=CARTESIAN_POINT('Ctrl Pts',(0.477768856872263,0.977025890449618,
1.1));
#21728=CARTESIAN_POINT('Ctrl Pts',(0.497468741075922,0.978719373910683,
1.1));
#21729=CARTESIAN_POINT('Ctrl Pts',(0.410427643322096,0.909072757750428,
1.1));
#21730=CARTESIAN_POINT('Ctrl Pts',(0.410598921732919,0.928815832685761,
1.09999369626122));
#21731=CARTESIAN_POINT('Ctrl Pts',(0.425924740546694,0.974670094016788,
1.09998538828789));
#21732=CARTESIAN_POINT('Ctrl Pts',(0.469296653719046,0.9992480682759,1.09999238300928));
#21733=CARTESIAN_POINT('Ctrl Pts',(0.495492436783666,1.00170924455528,1.1));
#21734=CARTESIAN_POINT('Ctrl Pts',(0.370309354350991,0.909072757750428,
1.08130565542949));
#21735=CARTESIAN_POINT('Ctrl Pts',(0.370756628991978,0.937276039918598,
1.0815946126737));
#21736=CARTESIAN_POINT('Ctrl Pts',(0.392976709797646,1.00253976529927,1.08203966084696));
#21737=CARTESIAN_POINT('Ctrl Pts',(0.45468128479604,1.03781409584644,1.08176448401818));
#21738=CARTESIAN_POINT('Ctrl Pts',(0.492065445269591,1.04157460937658,1.08141381101793));
#21739=CARTESIAN_POINT('Ctrl Pts',(0.354583574894625,0.909072757750428,
1.0415166534692));
#21740=CARTESIAN_POINT('Ctrl Pts',(0.354816047101877,0.940623786874923,
1.04226354472332));
#21741=CARTESIAN_POINT('Ctrl Pts',(0.379310481833935,1.01405872099115,1.04342813304911));
#21742=CARTESIAN_POINT('Ctrl Pts',(0.448832293580285,1.05343671745598,1.04270595335318));
#21743=CARTESIAN_POINT('Ctrl Pts',(0.490711556403977,1.05732407164794,1.04179769276967));
#21744=CARTESIAN_POINT('Ctrl Pts',(0.35367535976817,0.909072757750428,1.02418687649944));
#21745=CARTESIAN_POINT('Ctrl Pts',(0.353721546722556,0.940803974389028,
1.02506817608927));
#21746=CARTESIAN_POINT('Ctrl Pts',(0.378136805744942,1.01499479618886,1.02645106984513));
#21747=CARTESIAN_POINT('Ctrl Pts',(0.448470010609076,1.05461313661598,1.0255921777666));
#21748=CARTESIAN_POINT('Ctrl Pts',(0.490627822843887,1.05829812393464,1.02451933428366));
#21749=CARTESIAN_POINT('',(0.497468741075921,0.978719373910683,1.1));
#21750=CARTESIAN_POINT('',(0.490627822843887,1.05829812393464,1.02451933428366));
#21751=CARTESIAN_POINT('Origin',(0.497468741075921,0.978719373910683,1.02));
#21752=CARTESIAN_POINT('Ctrl Pts',(0.490627822843887,1.05829812393464,1.02451933428366));
#21753=CARTESIAN_POINT('Ctrl Pts',(0.448470010609076,1.05461313661598,1.0255921777666));
#21754=CARTESIAN_POINT('Ctrl Pts',(0.378136805744942,1.01499479618886,1.02645106984513));
#21755=CARTESIAN_POINT('Ctrl Pts',(0.353721546722556,0.940803974389028,
1.02506817608927));
#21756=CARTESIAN_POINT('Ctrl Pts',(0.35367535976817,0.909072757750428,1.02418687649944));
#21757=CARTESIAN_POINT('Ctrl Pts',(0.433565722548535,0.909072757750428,
1.1));
#21758=CARTESIAN_POINT('Ctrl Pts',(0.433565722548535,0.923902162481473,
1.1));
#21759=CARTESIAN_POINT('Ctrl Pts',(0.444925688709976,0.95855828847753,1.1));
#21760=CARTESIAN_POINT('Ctrl Pts',(0.477768856872263,0.977025890449618,
1.1));
#21761=CARTESIAN_POINT('Ctrl Pts',(0.497468741075922,0.978719373910683,
1.1));
#21762=CARTESIAN_POINT('Ctrl Pts',(0.497468741075922,0.978719373910683,
1.1));
#21763=CARTESIAN_POINT('Ctrl Pts',(1.89401780684616,1.09877250320817,1.1));
#21764=CARTESIAN_POINT('Ctrl Pts',(5.1654052076905,1.21987569230965,1.1));
#21765=CARTESIAN_POINT('Ctrl Pts',(8.43489748265729,1.08422939062092,1.1));
#21766=CARTESIAN_POINT('Ctrl Pts',(10.3006295894369,0.974894988741159,1.1));
#21767=CARTESIAN_POINT('Ctrl Pts',(0.495492436783665,1.00170924455528,1.1));
#21768=CARTESIAN_POINT('Ctrl Pts',(1.89278532112995,1.12186894072949,1.10000155140362));
#21769=CARTESIAN_POINT('Ctrl Pts',(5.16566149651331,1.24305592512388,1.09999870932828));
#21770=CARTESIAN_POINT('Ctrl Pts',(8.43598583180997,1.1073254346241,1.10000095186468));
#21771=CARTESIAN_POINT('Ctrl Pts',(10.3019806204244,0.997949597787003,1.1));
#21772=CARTESIAN_POINT('Ctrl Pts',(0.492066872450609,1.0415580073244,1.08139899772624));
#21773=CARTESIAN_POINT('Ctrl Pts',(1.89064106564166,1.16189659875033,1.08132757380279));
#21774=CARTESIAN_POINT('Ctrl Pts',(5.16610832342906,1.28323142649893,1.0812556832418));
#21775=CARTESIAN_POINT('Ctrl Pts',(8.43787502268472,1.14735362089424,1.08132197873404));
#21776=CARTESIAN_POINT('Ctrl Pts',(10.3043223112023,1.03790927738781,1.08136574244164));
#21777=CARTESIAN_POINT('Ctrl Pts',(0.490711556403977,1.05732407164794,1.04179769276967));
#21778=CARTESIAN_POINT('Ctrl Pts',(1.88980353393473,1.17765430418353,1.04161270124098));
#21779=CARTESIAN_POINT('Ctrl Pts',(5.16628155123749,1.29896165650174,1.04142536433641));
#21780=CARTESIAN_POINT('Ctrl Pts',(8.43861641093843,1.16310409863161,1.04159803213562));
#21781=CARTESIAN_POINT('Ctrl Pts',(10.3052465815697,1.05368144854439,1.04171131144128));
#21782=CARTESIAN_POINT('Ctrl Pts',(0.490627822843887,1.05829812393464,1.02451933428366));
#21783=CARTESIAN_POINT('Ctrl Pts',(1.88975348136405,1.17858515731652,1.02430082105127));
#21784=CARTESIAN_POINT('Ctrl Pts',(5.16629169073646,1.29984841142479,1.02407861909595));
#21785=CARTESIAN_POINT('Ctrl Pts',(8.43866044940558,1.1640312867702,1.02428334948326));
#21786=CARTESIAN_POINT('Ctrl Pts',(10.3053025283406,1.05463614976313,1.02441711227736));
#21787=CARTESIAN_POINT('Ctrl Pts',(10.3053025283406,1.05463614976313,1.02441711227736));
#21788=CARTESIAN_POINT('Ctrl Pts',(8.43866044940558,1.1640312867702,1.02428334948326));
#21789=CARTESIAN_POINT('Ctrl Pts',(5.16629169073646,1.29984841142479,1.02407861909595));
#21790=CARTESIAN_POINT('Ctrl Pts',(1.88975348136405,1.17858515731652,1.02430082105127));
#21791=CARTESIAN_POINT('Ctrl Pts',(0.490627822843887,1.05829812393464,1.02451933428366));
#21792=CARTESIAN_POINT('Ctrl Pts',(0.497468741075922,0.978719373910683,
1.1));
#21793=CARTESIAN_POINT('Ctrl Pts',(1.89401780684616,1.09877250320817,1.1));
#21794=CARTESIAN_POINT('Ctrl Pts',(5.1654052076905,1.21987569230965,1.1));
#21795=CARTESIAN_POINT('Ctrl Pts',(8.43489748265729,1.08422939062092,1.1));
#21796=CARTESIAN_POINT('Ctrl Pts',(10.3006295894369,0.974894988741159,1.1));
#21797=CARTESIAN_POINT('Origin',(0.347167001354737,-1.05283299864526,0.9));
#21798=CARTESIAN_POINT('',(0.347167001354737,0.915565952400859,0.9));
#21799=CARTESIAN_POINT('Ctrl Pts',(0.347167001354737,0.915565952400859,
0.9));
#21800=CARTESIAN_POINT('Ctrl Pts',(0.349336454142569,0.913401548092598,
0.941395625182189));
#21801=CARTESIAN_POINT('Ctrl Pts',(0.351505906947026,0.911237149868421,
0.982791250681617));
#21802=CARTESIAN_POINT('Ctrl Pts',(0.35367535976817,0.909072757750428,1.02418687649944));
#21803=CARTESIAN_POINT('',(0.347167001354737,-0.915565952400859,0.9));
#21804=CARTESIAN_POINT('',(0.347167001354737,-1.05283299864526,0.9));
#21805=CARTESIAN_POINT('Ctrl Pts',(0.35367535976817,-0.909072757750428,
1.02418687649944));
#21806=CARTESIAN_POINT('Ctrl Pts',(0.351505906947026,-0.911237149868421,
0.982791250681617));
#21807=CARTESIAN_POINT('Ctrl Pts',(0.349336454142569,-0.913401548092598,
0.941395625182188));
#21808=CARTESIAN_POINT('Ctrl Pts',(0.347167001354737,-0.915565952400859,
0.9));
#21809=CARTESIAN_POINT('Ctrl Pts',(0.346993933238254,0.915738617787778,
0.896697663613103));
#21810=CARTESIAN_POINT('Ctrl Pts',(0.349221075397351,0.913516658022686,
0.939194067573829));
#21811=CARTESIAN_POINT('Ctrl Pts',(0.351448217573968,0.911294704668933,
0.981690471868858));
#21812=CARTESIAN_POINT('Ctrl Pts',(0.35367535976817,0.909072757750428,1.02418687649944));
#21813=CARTESIAN_POINT('Ctrl Pts',(0.3471095194732,0.958036394339727,0.898903180361322));
#21814=CARTESIAN_POINT('Ctrl Pts',(0.349336694827029,0.955813381999015,
0.941399523267081));
#21815=CARTESIAN_POINT('Ctrl Pts',(0.351563761373338,0.953590428181058,
0.983895874971515));
#21816=CARTESIAN_POINT('Ctrl Pts',(0.353790936839104,0.951367426011707,
1.0263922183879));
#21817=CARTESIAN_POINT('Ctrl Pts',(0.38058410360499,1.03143776743275,0.900986703480571));
#21818=CARTESIAN_POINT('Ctrl Pts',(0.382809509257377,1.02921304595835,0.943483042387942));
#21819=CARTESIAN_POINT('Ctrl Pts',(0.38503494445329,1.0269883029847,0.985979378580876));
#21820=CARTESIAN_POINT('Ctrl Pts',(0.38726034587086,1.02476358729949,1.02847571797107));
#21821=CARTESIAN_POINT('Ctrl Pts',(0.452370958194108,1.06215086202928,0.898830373501354));
#21822=CARTESIAN_POINT('Ctrl Pts',(0.454593549384999,1.0599273359084,0.941326919294252));
#21823=CARTESIAN_POINT('Ctrl Pts',(0.456816159498039,1.05770384366995,0.983823465869046));
#21824=CARTESIAN_POINT('Ctrl Pts',(0.459038739297573,1.0554803259981,1.02632001264655));
#21825=CARTESIAN_POINT('Ctrl Pts',(0.48397786901498,1.06495020962439,0.897320291708494));
#21826=CARTESIAN_POINT('Ctrl Pts',(0.486199596570706,1.06272777115298,0.939816939358577));
#21827=CARTESIAN_POINT('Ctrl Pts',(0.488421317286976,1.06050533819043,0.982313587627295));
#21828=CARTESIAN_POINT('Ctrl Pts',(0.49064303113777,1.05828291075608,1.02481023651688));
#21829=CARTESIAN_POINT('',(0.484117964332956,1.06481006947648,0.9));
#21830=CARTESIAN_POINT('Ctrl Pts',(0.490627822843887,1.05829812393464,1.02451933428366));
#21831=CARTESIAN_POINT('Ctrl Pts',(0.488457876548035,1.06046876718106,0.983012888930869));
#21832=CARTESIAN_POINT('Ctrl Pts',(0.486287923702977,1.06263941570101,0.941506444170341));
#21833=CARTESIAN_POINT('Ctrl Pts',(0.484117964332956,1.06481006947648,0.9));
#21834=CARTESIAN_POINT('Ctrl Pts',(0.484117964332956,1.06481006947648,0.9));
#21835=CARTESIAN_POINT('Ctrl Pts',(0.473400395954556,1.06388989254567,0.899999999998067));
#21836=CARTESIAN_POINT('Ctrl Pts',(0.462835544435657,1.06178983909504,0.899998456484708));
#21837=CARTESIAN_POINT('Ctrl Pts',(0.452598733053303,1.05860868771556,0.899998088469989));
#21838=CARTESIAN_POINT('Ctrl Pts',(0.444242646677269,1.05601198306707,0.899997788067582));
#21839=CARTESIAN_POINT('Ctrl Pts',(0.436104524303727,1.05269365102958,0.899998236040192));
#21840=CARTESIAN_POINT('Ctrl Pts',(0.428287607266336,1.04868302953039,0.899999222960128));
#21841=CARTESIAN_POINT('Ctrl Pts',(0.418720381516705,1.0437743780639,0.900000430864189));
#21842=CARTESIAN_POINT('Ctrl Pts',(0.409734998843702,1.03788190267505,0.900002558923036));
#21843=CARTESIAN_POINT('Ctrl Pts',(0.401509364000825,1.03108161209803,0.900001877425249));
#21844=CARTESIAN_POINT('Ctrl Pts',(0.400282968007853,1.0300677269361,0.900001775817754));
#21845=CARTESIAN_POINT('Ctrl Pts',(0.399073506836177,1.02903357975146,0.900001605039306));
#21846=CARTESIAN_POINT('Ctrl Pts',(0.397881626738084,1.02797933950107,0.900001345423406));
#21847=CARTESIAN_POINT('Ctrl Pts',(0.39256805719391,1.02327938780652,0.900000188019117));
#21848=CARTESIAN_POINT('Ctrl Pts',(0.387603264903844,1.01818054769329,0.899997323013939));
#21849=CARTESIAN_POINT('Ctrl Pts',(0.383010638913681,1.01272978836618,0.899994456107983));
#21850=CARTESIAN_POINT('Ctrl Pts',(0.37606924632558,1.00449139480359,0.899990123005355));
#21851=CARTESIAN_POINT('Ctrl Pts',(0.370046554889952,0.995534526609835,
0.899986018340436));
#21852=CARTESIAN_POINT('Ctrl Pts',(0.3650033874046,0.986038739193365,0.899984773108821));
#21853=CARTESIAN_POINT('Ctrl Pts',(0.361794276996282,0.979996300523246,
0.899983980732651));
#21854=CARTESIAN_POINT('Ctrl Pts',(0.358982518390177,0.973734765189587,
0.899984261914926));
#21855=CARTESIAN_POINT('Ctrl Pts',(0.356593362150852,0.967295151176304,
0.899985518247832));
#21856=CARTESIAN_POINT('Ctrl Pts',(0.352862932284158,0.957240334312622,
0.899987479886722));
#21857=CARTESIAN_POINT('Ctrl Pts',(0.350196128254646,0.946848238515865,
0.899991935314924));
#21858=CARTESIAN_POINT('Ctrl Pts',(0.348668140386249,0.936282377262574,
0.899995621109591));
#21859=CARTESIAN_POINT('Ctrl Pts',(0.347678076093379,0.929436195976283,
0.89999800933123));
#21860=CARTESIAN_POINT('Ctrl Pts',(0.347167001781036,0.922516504287413,
0.899999999966543));
#21861=CARTESIAN_POINT('Ctrl Pts',(0.347167001354737,0.915565952400859,
0.9));
#21862=CARTESIAN_POINT('Ctrl Pts',(0.484117964332956,1.06481006947648,0.9));
#21863=CARTESIAN_POINT('Ctrl Pts',(0.486234267105875,1.06263480888061,0.94150644476122));
#21864=CARTESIAN_POINT('Ctrl Pts',(0.488350569878795,1.06045954828474,0.98301288952244));
#21865=CARTESIAN_POINT('Ctrl Pts',(0.490466872651714,1.05828428768887,1.02451933428366));
#21866=CARTESIAN_POINT('Ctrl Pts',(3.76001591476243,1.34606837492147,0.9));
#21867=CARTESIAN_POINT('Ctrl Pts',(3.76072193310095,1.3438931143256,0.94150644476122));
#21868=CARTESIAN_POINT('Ctrl Pts',(3.76142795143945,1.34171785372973,0.98301288952244));
#21869=CARTESIAN_POINT('Ctrl Pts',(3.76213396977796,1.33954259313386,1.02451933428366));
#21870=CARTESIAN_POINT('Ctrl Pts',(7.03591386519191,1.25287427294368,0.9));
#21871=CARTESIAN_POINT('Ctrl Pts',(7.03520959909601,1.25069901234781,0.94150644476122));
#21872=CARTESIAN_POINT('Ctrl Pts',(7.03450533300011,1.24852375175194,0.98301288952244));
#21873=CARTESIAN_POINT('Ctrl Pts',(7.03380106690421,1.24634849115607,1.02451933428366));
#21874=CARTESIAN_POINT('Ctrl Pts',(10.3118118156214,1.06114656258054,0.9));
#21875=CARTESIAN_POINT('Ctrl Pts',(10.3096972650911,1.05897130198467,0.94150644476122));
#21876=CARTESIAN_POINT('Ctrl Pts',(10.3075827145608,1.0567960413888,0.98301288952244));
#21877=CARTESIAN_POINT('Ctrl Pts',(10.3054681640305,1.05462078079293,1.02451933428366));
#21878=CARTESIAN_POINT('',(10.3118118156214,1.06114656258054,0.9));
#21879=CARTESIAN_POINT('Ctrl Pts',(10.3118118156214,1.06114656258054,0.9));
#21880=CARTESIAN_POINT('Ctrl Pts',(10.3096420485163,1.05897642099582,0.941472370325488));
#21881=CARTESIAN_POINT('Ctrl Pts',(10.3074722860834,1.05680628338526,0.982944741084089));
#21882=CARTESIAN_POINT('Ctrl Pts',(10.3053025283406,1.05463614976313,1.02441711227738));
#21883=CARTESIAN_POINT('Ctrl Pts',(0.484117964332956,1.06481006947648,0.9));
#21884=CARTESIAN_POINT('Ctrl Pts',(3.76001591476244,1.34606837492147,0.9));
#21885=CARTESIAN_POINT('Ctrl Pts',(7.03591386519191,1.25287427294368,0.9));
#21886=CARTESIAN_POINT('Ctrl Pts',(10.3118118156214,1.06114656258054,0.9));
#21887=CARTESIAN_POINT('Ctrl Pts',(10.3119584735067,1.0612932457764,0.897196819041737));
#21888=CARTESIAN_POINT('Ctrl Pts',(10.3097363069231,1.05907069570186,0.939670735378922));
#21889=CARTESIAN_POINT('Ctrl Pts',(10.3075141452397,1.0568481497954,0.982144652170355));
#21890=CARTESIAN_POINT('Ctrl Pts',(10.3052919884757,1.05462560807237,1.02461856941773));
#21891=CARTESIAN_POINT('Ctrl Pts',(10.3549577591382,1.05865952187103,0.899312513938921));
#21892=CARTESIAN_POINT('Ctrl Pts',(10.3527348026837,1.05643589667682,0.941786332790264));
#21893=CARTESIAN_POINT('Ctrl Pts',(10.3505118643323,1.05421236578444,0.984260157591605));
#21894=CARTESIAN_POINT('Ctrl Pts',(10.348288915563,1.05198874626302,1.02673397710222));
#21895=CARTESIAN_POINT('Ctrl Pts',(10.427476572305,1.0195555601276,0.90106705940868));
#21896=CARTESIAN_POINT('Ctrl Pts',(10.4252515051274,1.01733143721131,0.943540744474557));
#21897=CARTESIAN_POINT('Ctrl Pts',(10.423026434404,1.01510729429004,0.986014428272043));
#21898=CARTESIAN_POINT('Ctrl Pts',(10.4208013694594,1.01288317591826,1.02848811366363));
#21899=CARTESIAN_POINT('Ctrl Pts',(10.452914163627,0.944082648463888,0.89845127988914));
#21900=CARTESIAN_POINT('Ctrl Pts',(10.4506882024692,0.941859792143813,0.940924989850352));
#21901=CARTESIAN_POINT('Ctrl Pts',(10.4484622663099,0.939636927142988,0.983398700650476));
#21902=CARTESIAN_POINT('Ctrl Pts',(10.4462363051112,0.937414078664829,1.02587241101113));
#21903=CARTESIAN_POINT('Ctrl Pts',(10.453002503567,0.911777874403687,0.896765653419433));
#21904=CARTESIAN_POINT('Ctrl Pts',(10.4507765491346,0.909555555737009,0.939239394205133));
#21905=CARTESIAN_POINT('Ctrl Pts',(10.4485505946895,0.90733324168256,0.981713135231494));
#21906=CARTESIAN_POINT('Ctrl Pts',(10.4463246402318,0.905110932257975,1.02418687649944));
#21907=CARTESIAN_POINT('',(10.4528329986453,0.911608646352005,0.9));
#21908=CARTESIAN_POINT('Ctrl Pts',(10.4463246402318,0.905110932257975,1.02418687649944));
#21909=CARTESIAN_POINT('Ctrl Pts',(10.4484940930483,0.90727683256362,0.982791250770435));
#21910=CARTESIAN_POINT('Ctrl Pts',(10.4506635458528,0.909442737267073,0.941395625270907));
#21911=CARTESIAN_POINT('Ctrl Pts',(10.4528329986453,0.911608646352005,0.9));
#21912=CARTESIAN_POINT('Ctrl Pts',(10.4528329986453,0.911608646352005,0.9));
#21913=CARTESIAN_POINT('Ctrl Pts',(10.4528329984504,0.922365992175136,0.899999999995018));
#21914=CARTESIAN_POINT('Ctrl Pts',(10.4516419184466,0.933071221555305,0.899998396191737));
#21915=CARTESIAN_POINT('Ctrl Pts',(10.4493455883239,0.943542152407774,0.899997878793429));
#21916=CARTESIAN_POINT('Ctrl Pts',(10.4474685729764,0.952101068966945,0.899997455873155));
#21917=CARTESIAN_POINT('Ctrl Pts',(10.4448518647823,0.96050416098414,0.899997731911133));
#21918=CARTESIAN_POINT('Ctrl Pts',(10.4415172538375,0.968646108261598,0.899998556768105));
#21919=CARTESIAN_POINT('Ctrl Pts',(10.4374420364703,0.978596355981088,0.899999564823172));
#21920=CARTESIAN_POINT('Ctrl Pts',(10.4323389624922,0.988051909949456,0.900001510869465));
#21921=CARTESIAN_POINT('Ctrl Pts',(10.4262707314398,0.996829854811629,0.900000879982417));
#21922=CARTESIAN_POINT('Ctrl Pts',(10.4250393574459,0.998611087749148,0.900000751961929));
#21923=CARTESIAN_POINT('Ctrl Pts',(10.4237680854757,1.0003643483506,0.900000505994341));
#21924=CARTESIAN_POINT('Ctrl Pts',(10.4224572101159,1.00208797543426,0.90000009374416));
#21925=CARTESIAN_POINT('Ctrl Pts',(10.4185057422955,1.00728363107359,0.899998851068177));
#21926=CARTESIAN_POINT('Ctrl Pts',(10.4141947510749,1.0122104380758,0.899996136506224));
#21927=CARTESIAN_POINT('Ctrl Pts',(10.4095592300387,1.01684760353016,0.899993329936423));
#21928=CARTESIAN_POINT('Ctrl Pts',(10.4019420261375,1.02446750958049,0.899988718110854));
#21929=CARTESIAN_POINT('Ctrl Pts',(10.3935294957569,1.03122853977634,0.899984126639313));
#21930=CARTESIAN_POINT('Ctrl Pts',(10.3844977038391,1.03705893037027,0.899982514537369));
#21931=CARTESIAN_POINT('Ctrl Pts',(10.3781912117148,1.04113002863034,0.899981388879436));
#21932=CARTESIAN_POINT('Ctrl Pts',(10.3715817027072,1.04474676663118,0.899981626398985));
#21933=CARTESIAN_POINT('Ctrl Pts',(10.364720849853,1.04787222446317,0.899983147799038));
#21934=CARTESIAN_POINT('Ctrl Pts',(10.3549611185069,1.05231826483487,0.899985312027903));
#21935=CARTESIAN_POINT('Ctrl Pts',(10.34479058664,1.05572789097839,0.899990169054599));
#21936=CARTESIAN_POINT('Ctrl Pts',(10.3343672593286,1.0580160164031,0.899994394012168));
#21937=CARTESIAN_POINT('Ctrl Pts',(10.3269595157814,1.05964216185967,0.899997396642827));
#21938=CARTESIAN_POINT('Ctrl Pts',(10.3194233385871,1.06070108442786,0.899999999979614));
#21939=CARTESIAN_POINT('Ctrl Pts',(10.3118118156214,1.06114656258054,0.9));
#21940=CARTESIAN_POINT('Origin',(5.4,6.06940689584926E-17,1.1));
#21941=CARTESIAN_POINT('Origin',(10.4528329986453,1.05283299864526,0.9));
#21942=CARTESIAN_POINT('',(10.4528329986453,-0.911608646352005,0.9));
#21943=CARTESIAN_POINT('Ctrl Pts',(10.4528329986453,-0.911608646352005,
0.9));
#21944=CARTESIAN_POINT('Ctrl Pts',(10.4506635458528,-0.909442737267073,
0.941395625270908));
#21945=CARTESIAN_POINT('Ctrl Pts',(10.4484940930483,-0.907276832563621,
0.982791250770435));
#21946=CARTESIAN_POINT('Ctrl Pts',(10.4463246402318,-0.905110932257975,
1.02418687649944));
#21947=CARTESIAN_POINT('',(10.4528329986453,1.05283299864526,0.9));
#21948=CARTESIAN_POINT('Ctrl Pts',(0.483981659460312,-1.06494641796617,
0.897392794396587));
#21949=CARTESIAN_POINT('Ctrl Pts',(0.486202123526484,-1.0627252433871,0.939865274484676));
#21950=CARTESIAN_POINT('Ctrl Pts',(0.488422580760962,-1.06050407431064,
0.982337755190696));
#21951=CARTESIAN_POINT('Ctrl Pts',(0.49064303113777,-1.05828291075608,1.02481023651688));
#21952=CARTESIAN_POINT('Ctrl Pts',(0.441839113682364,-1.06121395205434,
0.899406236555586));
#21953=CARTESIAN_POINT('Ctrl Pts',(0.444060746976072,-1.05899130022525,
0.941878578466898));
#21954=CARTESIAN_POINT('Ctrl Pts',(0.446282352620465,-1.05676877539366,
0.984350928552248));
#21955=CARTESIAN_POINT('Ctrl Pts',(0.448503975350841,-1.05454613107877,
1.02682327135645));
#21956=CARTESIAN_POINT('Ctrl Pts',(0.371552730979752,-1.02159229167772,
0.901018138383736));
#21957=CARTESIAN_POINT('Ctrl Pts',(0.373777362914204,-1.01936901231721,
0.943490294374253));
#21958=CARTESIAN_POINT('Ctrl Pts',(0.376002007910301,-1.01714569791452,
0.985962447794501));
#21959=CARTESIAN_POINT('Ctrl Pts',(0.378226636819208,-1.01492242480963,
1.02843460423251));
#21960=CARTESIAN_POINT('Ctrl Pts',(0.347084422593647,-0.947458158036175,
0.898424303372123));
#21961=CARTESIAN_POINT('Ctrl Pts',(0.349310306978605,-0.945236691937326,
0.940896495998714));
#21962=CARTESIAN_POINT('Ctrl Pts',(0.351536158132471,-0.943015214174121,
0.983368689735046));
#21963=CARTESIAN_POINT('Ctrl Pts',(0.353762042571371,-0.940793758946387,
1.02584088291578));
#21964=CARTESIAN_POINT('Ctrl Pts',(0.346997732921341,-0.915734826946278,
0.896770165885443));
#21965=CARTESIAN_POINT('Ctrl Pts',(0.349223608519429,-0.913514130802309,
0.939242402422435));
#21966=CARTESIAN_POINT('Ctrl Pts',(0.351449484135016,-0.911293441062403,
0.981714639293352));
#21967=CARTESIAN_POINT('Ctrl Pts',(0.35367535976817,-0.909072757750428,
1.02418687649944));
#21968=CARTESIAN_POINT('',(0.484117964332957,-1.06481006947648,0.9));
#21969=CARTESIAN_POINT('Ctrl Pts',(0.347167001354737,-0.915565952400859,
0.9));
#21970=CARTESIAN_POINT('Ctrl Pts',(0.347167001618251,-0.926324952789844,
0.899999999993398));
#21971=CARTESIAN_POINT('Ctrl Pts',(0.348355267190738,-0.937032860435638,
0.899998616841383));
#21972=CARTESIAN_POINT('Ctrl Pts',(0.350648507770679,-0.947506517879914,
0.899998360166273));
#21973=CARTESIAN_POINT('Ctrl Pts',(0.352522341068278,-0.956064664041459,
0.899998150434084));
#21974=CARTESIAN_POINT('Ctrl Pts',(0.355135157141203,-0.964467130383873,
0.899998666502847));
#21975=CARTESIAN_POINT('Ctrl Pts',(0.358466575399326,-0.972608174091076,
0.89999965996049));
#21976=CARTESIAN_POINT('Ctrl Pts',(0.362538734686669,-0.982559379305286,
0.900000874313493));
#21977=CARTESIAN_POINT('Ctrl Pts',(0.367640276064737,-0.992015301694373,
0.90000291775694));
#21978=CARTESIAN_POINT('Ctrl Pts',(0.373711018494534,-1.00079214745216,
0.900002098461893));
#21979=CARTESIAN_POINT('Ctrl Pts',(0.3746124109217,-1.00209534593109,0.900001976811805));
#21980=CARTESIAN_POINT('Ctrl Pts',(0.375535256028145,-1.00338353399439,
0.900001785555943));
#21981=CARTESIAN_POINT('Ctrl Pts',(0.376479443106529,-1.00465606108108,
0.900001505529245));
#21982=CARTESIAN_POINT('Ctrl Pts',(0.380715143239362,-1.01036472123275,
0.900000249306668));
#21983=CARTESIAN_POINT('Ctrl Pts',(0.385379830512911,-1.01575881671377,
0.899997265714102));
#21984=CARTESIAN_POINT('Ctrl Pts',(0.390428509023093,-1.02081078987204,
0.899994288896867));
#21985=CARTESIAN_POINT('Ctrl Pts',(0.398043974952909,-1.02843122547464,
0.899989798642598));
#21986=CARTESIAN_POINT('Ctrl Pts',(0.406453848296673,-1.0351976329321,0.899985566096));
#21987=CARTESIAN_POINT('Ctrl Pts',(0.415484607049401,-1.04103374418621,
0.899984276342262));
#21988=CARTESIAN_POINT('Ctrl Pts',(0.421222938370041,-1.04474213026064,
0.899983456806));
#21989=CARTESIAN_POINT('Ctrl Pts',(0.427212893823218,-1.04807424787086,
0.899983742291921));
#21990=CARTESIAN_POINT('Ctrl Pts',(0.433415948881005,-1.05100146303553,
0.899985033489932));
#21991=CARTESIAN_POINT('Ctrl Pts',(0.443112479013355,-1.05557724541753,
0.899987051872858));
#21992=CARTESIAN_POINT('Ctrl Pts',(0.453235937005982,-1.05912207412747,
0.899991654125809));
#21993=CARTESIAN_POINT('Ctrl Pts',(0.463629957379397,-1.06154692150368,
0.899995467994069));
#21994=CARTESIAN_POINT('Ctrl Pts',(0.470358492676306,-1.06311663856929,
0.899997936889288));
#21995=CARTESIAN_POINT('Ctrl Pts',(0.477201035001208,-1.06421620326297,
0.899999999975707));
#21996=CARTESIAN_POINT('Ctrl Pts',(0.484117964332956,-1.06481006947648,
0.9));
#21997=CARTESIAN_POINT('Ctrl Pts',(0.484117964332956,-1.06481006947648,
0.9));
#21998=CARTESIAN_POINT('Ctrl Pts',(0.486287923702977,-1.06263941570101,
0.941506444170342));
#21999=CARTESIAN_POINT('Ctrl Pts',(0.488457876548035,-1.06046876718106,
0.983012888930867));
#22000=CARTESIAN_POINT('Ctrl Pts',(0.490627822843887,-1.05829812393464,
1.02451933428366));
#22001=CARTESIAN_POINT('Ctrl Pts',(10.453005262311,-0.911780628641665,0.896713013448579));
#22002=CARTESIAN_POINT('Ctrl Pts',(10.4507783882972,-0.90955739189185,0.939204300891032));
#22003=CARTESIAN_POINT('Ctrl Pts',(10.4485515142709,-0.907334159758067,
0.981695588574343));
#22004=CARTESIAN_POINT('Ctrl Pts',(10.4463246402318,-0.905110932257975,
1.02418687649944));
#22005=CARTESIAN_POINT('Ctrl Pts',(10.4528874757217,-0.954853661617318,
0.898960515458773));
#22006=CARTESIAN_POINT('Ctrl Pts',(10.4506605772126,-0.952629688741643,
0.941451759962203));
#22007=CARTESIAN_POINT('Ctrl Pts',(10.4484337586651,-0.950405759674028,
0.983943010977281));
#22008=CARTESIAN_POINT('Ctrl Pts',(10.4462068600709,-0.948181794133781,
1.02643425584837));
#22009=CARTESIAN_POINT('Ctrl Pts',(10.4180804799687,-1.02952167699519,0.901043151378082));
#22010=CARTESIAN_POINT('Ctrl Pts',(10.4158548456208,-1.02729651565793,0.943534394542847));
#22011=CARTESIAN_POINT('Ctrl Pts',(10.413629193759,-1.02507134540722,0.986025636297673));
#22012=CARTESIAN_POINT('Ctrl Pts',(10.4114035625395,-1.02284618829514,1.02851687981561));
#22013=CARTESIAN_POINT('Ctrl Pts',(10.3442106925096,-1.05932070834318,0.898730950115076));
#22014=CARTESIAN_POINT('Ctrl Pts',(10.3419870251366,-1.05709644901815,0.941222341385074));
#22015=CARTESIAN_POINT('Ctrl Pts',(10.3397633429135,-1.0548722146549,0.983713733185165));
#22016=CARTESIAN_POINT('Ctrl Pts',(10.3375396837912,-1.05264796171536,1.0262051251811));
#22017=CARTESIAN_POINT('Ctrl Pts',(10.3119612275562,-1.06129600030118,0.897144178853313));
#22018=CARTESIAN_POINT('Ctrl Pts',(10.309738142952,-1.05907253204827,0.939635641919599));
#22019=CARTESIAN_POINT('Ctrl Pts',(10.3075150632522,-1.05684906796687,0.982127105440503));
#22020=CARTESIAN_POINT('Ctrl Pts',(10.3052919884757,-1.05462560807237,1.02461856941773));
#22021=CARTESIAN_POINT('',(10.3118118156214,-1.06114656258054,0.9));
#22022=CARTESIAN_POINT('Ctrl Pts',(10.3053025283406,-1.05463614976313,1.02441711227736));
#22023=CARTESIAN_POINT('Ctrl Pts',(10.3074722860834,-1.05680628338526,0.982944741084074));
#22024=CARTESIAN_POINT('Ctrl Pts',(10.3096420485163,-1.05897642099582,0.941472370325483));
#22025=CARTESIAN_POINT('Ctrl Pts',(10.3118118156214,-1.06114656258054,0.900000000000001));
#22026=CARTESIAN_POINT('Ctrl Pts',(10.3118118156214,-1.06114656258054,0.900000000000001));
#22027=CARTESIAN_POINT('Ctrl Pts',(10.322549369014,-1.06051812817027,0.899999999998837));
#22028=CARTESIAN_POINT('Ctrl Pts',(10.3331651969327,-1.05870347076406,0.899998279675625));
#22029=CARTESIAN_POINT('Ctrl Pts',(10.3434824690201,-1.05579899810317,0.899997678781422));
#22030=CARTESIAN_POINT('Ctrl Pts',(10.3519099591122,-1.05342652848477,0.899997187951103));
#22031=CARTESIAN_POINT('Ctrl Pts',(10.3601388923794,-1.05032564389788,0.899997411230107));
#22032=CARTESIAN_POINT('Ctrl Pts',(10.368065652211,-1.04652424300033,0.899998227267474));
#22033=CARTESIAN_POINT('Ctrl Pts',(10.3777613500057,-1.04187452040475,0.89999922541197));
#22034=CARTESIAN_POINT('Ctrl Pts',(10.3869029298231,-1.0362271920453,0.900001226887481));
#22035=CARTESIAN_POINT('Ctrl Pts',(10.3953114913929,-1.02965576012812,0.900000692598515));
#22036=CARTESIAN_POINT('Ctrl Pts',(10.3970212347867,-1.0283195669856,0.900000583959597));
#22037=CARTESIAN_POINT('Ctrl Pts',(10.3987005924826,-1.02694501523934,0.900000358370781));
#22038=CARTESIAN_POINT('Ctrl Pts',(10.4003479139729,-1.02553250004787,0.899999966744969));
#22039=CARTESIAN_POINT('Ctrl Pts',(10.4052955867552,-1.02129005981461,0.899998790510468));
#22040=CARTESIAN_POINT('Ctrl Pts',(10.4099546972526,-1.01670546321193,0.899996154952331));
#22041=CARTESIAN_POINT('Ctrl Pts',(10.4143066574475,-1.01181472964029,0.899993423989004));
#22042=CARTESIAN_POINT('Ctrl Pts',(10.4214686344271,-1.00376609875091,0.899988929670213));
#22043=CARTESIAN_POINT('Ctrl Pts',(10.4277268376922,-0.994973664259555,
0.899984438878373));
#22044=CARTESIAN_POINT('Ctrl Pts',(10.4330201329469,-0.98561748607337,0.899982870029797));
#22045=CARTESIAN_POINT('Ctrl Pts',(10.4367196060238,-0.979078472540648,
0.89998177356478));
#22046=CARTESIAN_POINT('Ctrl Pts',(10.4399470827666,-0.972263038755176,
0.89998201356482));
#22047=CARTESIAN_POINT('Ctrl Pts',(10.4426687152005,-0.965225084739993,
0.899983510148066));
#22048=CARTESIAN_POINT('Ctrl Pts',(10.4465375225522,-0.955220615401818,
0.899985637544916));
#22049=CARTESIAN_POINT('Ctrl Pts',(10.4493477346146,-0.944866529467853,
0.899990392295554));
#22050=CARTESIAN_POINT('Ctrl Pts',(10.4510237312406,-0.934325606572895,
0.899994522211612));
#22051=CARTESIAN_POINT('Ctrl Pts',(10.452215546318,-0.926829869027477,0.899997459029114));
#22052=CARTESIAN_POINT('Ctrl Pts',(10.452832998309,-0.919238945488459,0.899999999973399));
#22053=CARTESIAN_POINT('Ctrl Pts',(10.4528329986453,-0.911608646352005,
0.9));
#22054=CARTESIAN_POINT('Origin',(5.4,0.,0.9));
#22055=CARTESIAN_POINT('Ctrl Pts',(10.3118118156214,-1.06114656258054,0.9));
#22056=CARTESIAN_POINT('Ctrl Pts',(7.03591386519191,-1.25287427294368,0.9));
#22057=CARTESIAN_POINT('Ctrl Pts',(3.76001591476243,-1.34606837492147,0.9));
#22058=CARTESIAN_POINT('Ctrl Pts',(0.484117964332957,-1.06481006947648,
0.9));
#22059=CARTESIAN_POINT('Ctrl Pts',(10.3118118156214,-1.06114656258054,0.9));
#22060=CARTESIAN_POINT('Ctrl Pts',(10.3096972650911,-1.05897130198467,0.94150644476122));
#22061=CARTESIAN_POINT('Ctrl Pts',(10.3075827145608,-1.0567960413888,0.98301288952244));
#22062=CARTESIAN_POINT('Ctrl Pts',(10.3054681640305,-1.05462078079293,1.02451933428366));
#22063=CARTESIAN_POINT('Ctrl Pts',(7.03591386519191,-1.25287427294368,0.9));
#22064=CARTESIAN_POINT('Ctrl Pts',(7.03520959909601,-1.25069901234781,0.94150644476122));
#22065=CARTESIAN_POINT('Ctrl Pts',(7.03450533300011,-1.24852375175194,0.98301288952244));
#22066=CARTESIAN_POINT('Ctrl Pts',(7.03380106690421,-1.24634849115607,1.02451933428366));
#22067=CARTESIAN_POINT('Ctrl Pts',(3.76001591476244,-1.34606837492147,0.9));
#22068=CARTESIAN_POINT('Ctrl Pts',(3.76072193310095,-1.3438931143256,0.94150644476122));
#22069=CARTESIAN_POINT('Ctrl Pts',(3.76142795143946,-1.34171785372973,0.98301288952244));
#22070=CARTESIAN_POINT('Ctrl Pts',(3.76213396977796,-1.33954259313386,1.02451933428366));
#22071=CARTESIAN_POINT('Ctrl Pts',(0.484117964332957,-1.06481006947648,
0.9));
#22072=CARTESIAN_POINT('Ctrl Pts',(0.486234267105876,-1.06263480888061,
0.94150644476122));
#22073=CARTESIAN_POINT('Ctrl Pts',(0.488350569878795,-1.06045954828474,
0.98301288952244));
#22074=CARTESIAN_POINT('Ctrl Pts',(0.490466872651714,-1.05828428768887,
1.02451933428366));
#22075=CARTESIAN_POINT('',(0.,0.,0.));
#22076=CARTESIAN_POINT('',(0.,0.,0.));
#22077=CARTESIAN_POINT('',(2.,0.,0.6));
#22078=CARTESIAN_POINT('',(2.,0.,-0.84));
#22079=CARTESIAN_POINT('',(0.,0.,0.));
#22080=CARTESIAN_POINT('',(8.8,0.,0.6));
#22081=CARTESIAN_POINT('',(8.8,0.,-0.84));
#22082=CARTESIAN_POINT('',(0.,0.,0.));
#22083=CARTESIAN_POINT('',(0.,0.,0.));
#22084=CARTESIAN_POINT('Origin',(0.,0.,0.));
#22085=CARTESIAN_POINT('',(-0.41,-5.02105187650415E-17,0.1));
#22086=CARTESIAN_POINT('Origin',(0.,0.,0.1));
#22087=CARTESIAN_POINT('',(-0.41,-5.02105187650415E-17,0.));
#22088=CARTESIAN_POINT('',(-0.41,-5.02105187650415E-17,0.));
#22089=CARTESIAN_POINT('Origin',(0.,0.,0.));
#22090=CARTESIAN_POINT('Origin',(0.,0.,0.));
#22091=CARTESIAN_POINT('',(-0.6,-7.34788079488412E-17,0.1));
#22092=CARTESIAN_POINT('Origin',(0.,0.,0.1));
#22093=CARTESIAN_POINT('',(-0.6,-7.34788079488412E-17,0.));
#22094=CARTESIAN_POINT('',(-0.6,-7.34788079488412E-17,0.));
#22095=CARTESIAN_POINT('Origin',(0.,0.,0.));
#22096=CARTESIAN_POINT('Origin',(0.,0.,0.1));
#22097=CARTESIAN_POINT('Origin',(0.,0.,0.));
#22098=CARTESIAN_POINT('',(0.,0.,0.));
#22099=CARTESIAN_POINT('',(4.,-2.5,0.3));
#22100=CARTESIAN_POINT('',(2.57942197801717E-55,-1.73230948457749E-55,-3.67983215933355E-78));
#22101=CARTESIAN_POINT('',(0.,0.,0.));
#22102=CARTESIAN_POINT('',(0.,0.,0.6));
#22103=CARTESIAN_POINT('',(0.,0.,0.7));
#22104=CARTESIAN_POINT('',(2.56868392342393,3.95624353415502,-0.3));
#22105=CARTESIAN_POINT('',(0.,0.,-0.7));
#22106=UNCERTAINTY_MEASURE_WITH_UNIT(LENGTH_MEASURE(0.001),#22130,
'DISTANCE_ACCURACY_VALUE',
'Maximum model space distance between geometric entities at asserted c
onnectivities');
#22107=UNCERTAINTY_MEASURE_WITH_UNIT(LENGTH_MEASURE(0.001),#22130,
'DISTANCE_ACCURACY_VALUE',
'Maximum model space distance between geometric entities at asserted c
onnectivities');
#22108=UNCERTAINTY_MEASURE_WITH_UNIT(LENGTH_MEASURE(0.001),#22130,
'DISTANCE_ACCURACY_VALUE',
'Maximum model space distance between geometric entities at asserted c
onnectivities');
#22109=UNCERTAINTY_MEASURE_WITH_UNIT(LENGTH_MEASURE(0.001),#22130,
'DISTANCE_ACCURACY_VALUE',
'Maximum model space distance between geometric entities at asserted c
onnectivities');
#22110=UNCERTAINTY_MEASURE_WITH_UNIT(LENGTH_MEASURE(0.001),#22130,
'DISTANCE_ACCURACY_VALUE',
'Maximum model space distance between geometric entities at asserted c
onnectivities');
#22111=UNCERTAINTY_MEASURE_WITH_UNIT(LENGTH_MEASURE(0.001),#22130,
'DISTANCE_ACCURACY_VALUE',
'Maximum model space distance between geometric entities at asserted c
onnectivities');
#22112=UNCERTAINTY_MEASURE_WITH_UNIT(LENGTH_MEASURE(0.001),#22130,
'DISTANCE_ACCURACY_VALUE',
'Maximum model space distance between geometric entities at asserted c
onnectivities');
#22113=UNCERTAINTY_MEASURE_WITH_UNIT(LENGTH_MEASURE(0.001),#22130,
'DISTANCE_ACCURACY_VALUE',
'Maximum model space distance between geometric entities at asserted c
onnectivities');
#22114=UNCERTAINTY_MEASURE_WITH_UNIT(LENGTH_MEASURE(0.001),#22130,
'DISTANCE_ACCURACY_VALUE',
'Maximum model space distance between geometric entities at asserted c
onnectivities');
#22115=UNCERTAINTY_MEASURE_WITH_UNIT(LENGTH_MEASURE(0.001),#22130,
'DISTANCE_ACCURACY_VALUE',
'Maximum model space distance between geometric entities at asserted c
onnectivities');
#22116=UNCERTAINTY_MEASURE_WITH_UNIT(LENGTH_MEASURE(0.001),#22130,
'DISTANCE_ACCURACY_VALUE',
'Maximum model space distance between geometric entities at asserted c
onnectivities');
#22117=UNCERTAINTY_MEASURE_WITH_UNIT(LENGTH_MEASURE(0.001),#22130,
'DISTANCE_ACCURACY_VALUE',
'Maximum model space distance between geometric entities at asserted c
onnectivities');
#22118=(
GEOMETRIC_REPRESENTATION_CONTEXT(3)
GLOBAL_UNCERTAINTY_ASSIGNED_CONTEXT((#22106))
GLOBAL_UNIT_ASSIGNED_CONTEXT((#22130,#22132,#22133))
REPRESENTATION_CONTEXT('','3D')
);
#22119=(
GEOMETRIC_REPRESENTATION_CONTEXT(3)
GLOBAL_UNCERTAINTY_ASSIGNED_CONTEXT((#22107))
GLOBAL_UNIT_ASSIGNED_CONTEXT((#22130,#22132,#22133))
REPRESENTATION_CONTEXT('','3D')
);
#22120=(
GEOMETRIC_REPRESENTATION_CONTEXT(3)
GLOBAL_UNCERTAINTY_ASSIGNED_CONTEXT((#22108))
GLOBAL_UNIT_ASSIGNED_CONTEXT((#22130,#22132,#22133))
REPRESENTATION_CONTEXT('','3D')
);
#22121=(
GEOMETRIC_REPRESENTATION_CONTEXT(3)
GLOBAL_UNCERTAINTY_ASSIGNED_CONTEXT((#22109))
GLOBAL_UNIT_ASSIGNED_CONTEXT((#22130,#22132,#22133))
REPRESENTATION_CONTEXT('','3D')
);
#22122=(
GEOMETRIC_REPRESENTATION_CONTEXT(3)
GLOBAL_UNCERTAINTY_ASSIGNED_CONTEXT((#22110))
GLOBAL_UNIT_ASSIGNED_CONTEXT((#22130,#22132,#22133))
REPRESENTATION_CONTEXT('','3D')
);
#22123=(
GEOMETRIC_REPRESENTATION_CONTEXT(3)
GLOBAL_UNCERTAINTY_ASSIGNED_CONTEXT((#22111))
GLOBAL_UNIT_ASSIGNED_CONTEXT((#22130,#22132,#22133))
REPRESENTATION_CONTEXT('','3D')
);
#22124=(
GEOMETRIC_REPRESENTATION_CONTEXT(3)
GLOBAL_UNCERTAINTY_ASSIGNED_CONTEXT((#22112))
GLOBAL_UNIT_ASSIGNED_CONTEXT((#22130,#22132,#22133))
REPRESENTATION_CONTEXT('','3D')
);
#22125=(
GEOMETRIC_REPRESENTATION_CONTEXT(3)
GLOBAL_UNCERTAINTY_ASSIGNED_CONTEXT((#22113))
GLOBAL_UNIT_ASSIGNED_CONTEXT((#22130,#22132,#22133))
REPRESENTATION_CONTEXT('','3D')
);
#22126=(
GEOMETRIC_REPRESENTATION_CONTEXT(3)
GLOBAL_UNCERTAINTY_ASSIGNED_CONTEXT((#22114))
GLOBAL_UNIT_ASSIGNED_CONTEXT((#22130,#22132,#22133))
REPRESENTATION_CONTEXT('','3D')
);
#22127=(
GEOMETRIC_REPRESENTATION_CONTEXT(3)
GLOBAL_UNCERTAINTY_ASSIGNED_CONTEXT((#22115))
GLOBAL_UNIT_ASSIGNED_CONTEXT((#22130,#22132,#22133))
REPRESENTATION_CONTEXT('','3D')
);
#22128=(
GEOMETRIC_REPRESENTATION_CONTEXT(3)
GLOBAL_UNCERTAINTY_ASSIGNED_CONTEXT((#22116))
GLOBAL_UNIT_ASSIGNED_CONTEXT((#22130,#22132,#22133))
REPRESENTATION_CONTEXT('','3D')
);
#22129=(
GEOMETRIC_REPRESENTATION_CONTEXT(3)
GLOBAL_UNCERTAINTY_ASSIGNED_CONTEXT((#22117))
GLOBAL_UNIT_ASSIGNED_CONTEXT((#22130,#22132,#22133))
REPRESENTATION_CONTEXT('','3D')
);
#22130=(
LENGTH_UNIT()
NAMED_UNIT(*)
SI_UNIT(.CENTI.,.METRE.)
);
#22131=(
LENGTH_UNIT()
NAMED_UNIT(*)
SI_UNIT($,.METRE.)
);
#22132=(
NAMED_UNIT(*)
PLANE_ANGLE_UNIT()
SI_UNIT($,.RADIAN.)
);
#22133=(
NAMED_UNIT(*)
SI_UNIT($,.STERADIAN.)
SOLID_ANGLE_UNIT()
);
#22134=SHAPE_DEFINITION_REPRESENTATION(#22145,#22172);
#22135=SHAPE_DEFINITION_REPRESENTATION(#22146,#22173);
#22136=SHAPE_DEFINITION_REPRESENTATION(#22147,#22174);
#22137=SHAPE_DEFINITION_REPRESENTATION(#22148,#22175);
#22138=SHAPE_DEFINITION_REPRESENTATION(#22149,#22176);
#22139=SHAPE_DEFINITION_REPRESENTATION(#22150,#22177);
#22140=SHAPE_DEFINITION_REPRESENTATION(#22151,#22178);
#22141=SHAPE_DEFINITION_REPRESENTATION(#22152,#22179);
#22142=SHAPE_DEFINITION_REPRESENTATION(#22153,#22180);
#22143=SHAPE_DEFINITION_REPRESENTATION(#22154,#22181);
#22144=SHAPE_DEFINITION_REPRESENTATION(#22163,#22182);
#22145=PRODUCT_DEFINITION_SHAPE('',$,#22184);
#22146=PRODUCT_DEFINITION_SHAPE('',$,#22185);
#22147=PRODUCT_DEFINITION_SHAPE('',$,#22186);
#22148=PRODUCT_DEFINITION_SHAPE('',$,#22187);
#22149=PRODUCT_DEFINITION_SHAPE('',$,#22188);
#22150=PRODUCT_DEFINITION_SHAPE('',$,#22189);
#22151=PRODUCT_DEFINITION_SHAPE('',$,#22190);
#22152=PRODUCT_DEFINITION_SHAPE('',$,#22191);
#22153=PRODUCT_DEFINITION_SHAPE('',$,#22192);
#22154=PRODUCT_DEFINITION_SHAPE('',$,#22193);
#22155=PRODUCT_DEFINITION_SHAPE($,$,#59);
#22156=PRODUCT_DEFINITION_SHAPE($,$,#60);
#22157=PRODUCT_DEFINITION_SHAPE($,$,#61);
#22158=PRODUCT_DEFINITION_SHAPE($,$,#62);
#22159=PRODUCT_DEFINITION_SHAPE($,$,#63);
#22160=PRODUCT_DEFINITION_SHAPE($,$,#64);
#22161=PRODUCT_DEFINITION_SHAPE($,$,#65);
#22162=PRODUCT_DEFINITION_SHAPE($,$,#66);
#22163=PRODUCT_DEFINITION_SHAPE('',$,#22194);
#22164=PRODUCT_DEFINITION_SHAPE($,$,#67);
#22165=PRODUCT_DEFINITION_SHAPE($,$,#68);
#22166=PRODUCT_DEFINITION_SHAPE($,$,#69);
#22167=PRODUCT_DEFINITION_SHAPE($,$,#70);
#22168=PRODUCT_DEFINITION_SHAPE($,$,#71);
#22169=PRODUCT_DEFINITION_SHAPE($,$,#72);
#22170=PRODUCT_DEFINITION_SHAPE($,$,#73);
#22171=PRODUCT_DEFINITION_SHAPE($,$,#74);
#22172=SHAPE_REPRESENTATION('',(#8912,#9492,#9493,#9494,#9495,#9496,#9497,
#9498,#9499),#22118);
#22173=SHAPE_REPRESENTATION('',(#8913),#22119);
#22174=SHAPE_REPRESENTATION('',(#9058),#22120);
#22175=SHAPE_REPRESENTATION('',(#9076),#22121);
#22176=SHAPE_REPRESENTATION('',(#9087,#9475,#9476,#9477,#9478,#9479,#9480,
#9481,#9482),#22122);
#22177=SHAPE_REPRESENTATION('',(#9088),#22123);
#22178=SHAPE_REPRESENTATION('',(#9198),#22124);
#22179=SHAPE_REPRESENTATION('',(#9314),#22125);
#22180=SHAPE_REPRESENTATION('',(#9396),#22126);
#22181=SHAPE_REPRESENTATION('',(#9422),#22127);
#22182=SHAPE_REPRESENTATION('',(#9483),#22128);
#22183=PRODUCT_DEFINITION_CONTEXT('part definition',#22218,'design');
#22184=PRODUCT_DEFINITION('2026-11-12-00-52-51-422','TAS-009',#22195,#22183);
#22185=PRODUCT_DEFINITION('Forged jaw and handle',
'Forged jaw and handle',#22196,#22183);
#22186=PRODUCT_DEFINITION('Shoulder pivot pin','Shoulder pivot pin',#22197,
#22183);
#22187=PRODUCT_DEFINITION('Pivot retaining ring','Pivot retaining ring',
#22198,#22183);
#22188=PRODUCT_DEFINITION('Fiber_Grip_Handle','Fiber_Grip_Handle',#22199,
#22183);
#22189=PRODUCT_DEFINITION('2026-11-10-05-10-49-232',
'Upper structural shell',#22200,#22183);
#22190=PRODUCT_DEFINITION('2026-11-10-05-10-49-236',
'Lower structural shell',#22201,#22183);
#22191=PRODUCT_DEFINITION('2026-11-10-05-10-49-240',
'Socket head cap screw M3x16',#22202,#22183);
#22192=PRODUCT_DEFINITION('2026-11-10-05-10-49-241','Hex nut M3',#22203,
#22183);
#22193=PRODUCT_DEFINITION('2026-11-10-05-10-49-242','Soft grip layer',#22204,
#22183);
#22194=PRODUCT_DEFINITION('Pivot thrust washer','Pivot thrust washer',#22205,
#22183);
#22195=PRODUCT_DEFINITION_FORMATION('',$,#22220);
#22196=PRODUCT_DEFINITION_FORMATION('',$,#22221);
#22197=PRODUCT_DEFINITION_FORMATION('',$,#22222);
#22198=PRODUCT_DEFINITION_FORMATION('',$,#22223);
#22199=PRODUCT_DEFINITION_FORMATION('',$,#22224);
#22200=PRODUCT_DEFINITION_FORMATION('',$,#22225);
#22201=PRODUCT_DEFINITION_FORMATION('',$,#22226);
#22202=PRODUCT_DEFINITION_FORMATION('',$,#22227);
#22203=PRODUCT_DEFINITION_FORMATION('',$,#22228);
#22204=PRODUCT_DEFINITION_FORMATION('',$,#22229);
#22205=PRODUCT_DEFINITION_FORMATION('',$,#22230);
#22206=PRODUCT_RELATED_PRODUCT_CATEGORY('TAS-009','TAS-009',(#22220));
#22207=PRODUCT_RELATED_PRODUCT_CATEGORY('Forged jaw and handle',
'Forged jaw and handle',(#22221));
#22208=PRODUCT_RELATED_PRODUCT_CATEGORY('Shoulder pivot pin',
'Shoulder pivot pin',(#22222));
#22209=PRODUCT_RELATED_PRODUCT_CATEGORY('Pivot retaining ring',
'Pivot retaining ring',(#22223));
#22210=PRODUCT_RELATED_PRODUCT_CATEGORY('Fiber_Grip_Handle',
'Fiber_Grip_Handle',(#22224));
#22211=PRODUCT_RELATED_PRODUCT_CATEGORY('Upper structural shell',
'Upper structural shell',(#22225));
#22212=PRODUCT_RELATED_PRODUCT_CATEGORY('Lower structural shell',
'Lower structural shell',(#22226));
#22213=PRODUCT_RELATED_PRODUCT_CATEGORY('Socket head cap screw M3x16',
'Socket head cap screw M3x16',(#22227));
#22214=PRODUCT_RELATED_PRODUCT_CATEGORY('Hex nut M3','Hex nut M3',(#22228));
#22215=PRODUCT_RELATED_PRODUCT_CATEGORY('Soft grip layer',
'Soft grip layer',(#22229));
#22216=PRODUCT_RELATED_PRODUCT_CATEGORY('Pivot thrust washer',
'Pivot thrust washer',(#22230));
#22217=APPLICATION_PROTOCOL_DEFINITION('international standard',
'automotive_design',2009,#22218);
#22218=APPLICATION_CONTEXT(
'Core Data for Automotive Mechanical Design Process');
#22219=PRODUCT_CONTEXT('part definition',#22218,'mechanical');
#22220=PRODUCT('2026-11-12-00-52-51-422','TAS-009',$,(#22219));
#22221=PRODUCT('Forged jaw and handle','Forged jaw and handle',$,(#22219));
#22222=PRODUCT('Shoulder pivot pin','Shoulder pivot pin',$,(#22219));
#22223=PRODUCT('Pivot retaining ring','Pivot retaining ring',$,(#22219));
#22224=PRODUCT('Fiber_Grip_Handle','Fiber_Grip_Handle',$,(#22219));
#22225=PRODUCT('2026-11-10-05-10-49-232','Upper structural shell',$,(#22219));
#22226=PRODUCT('2026-11-10-05-10-49-236','Lower structural shell',$,(#22219));
#22227=PRODUCT('2026-11-10-05-10-49-240','Socket head cap screw M3x16',
$,(#22219));
#22228=PRODUCT('2026-11-10-05-10-49-241','Hex nut M3',$,(#22219));
#22229=PRODUCT('2026-11-10-05-10-49-242','Soft grip layer',$,(#22219));
#22230=PRODUCT('Pivot thrust washer','Pivot thrust washer',$,(#22219));
#22231=PRESENTATION_STYLE_ASSIGNMENT((#22239));
#22232=PRESENTATION_STYLE_ASSIGNMENT((#22240));
#22233=PRESENTATION_STYLE_ASSIGNMENT((#22241));
#22234=PRESENTATION_STYLE_ASSIGNMENT((#22242));
#22235=PRESENTATION_STYLE_ASSIGNMENT((#22243));
#22236=PRESENTATION_STYLE_ASSIGNMENT((#22244));
#22237=PRESENTATION_STYLE_ASSIGNMENT((#22245));
#22238=PRESENTATION_STYLE_ASSIGNMENT((#22246));
#22239=SURFACE_STYLE_USAGE(.BOTH.,#22247);
#22240=SURFACE_STYLE_USAGE(.BOTH.,#22248);
#22241=SURFACE_STYLE_USAGE(.BOTH.,#22249);
#22242=SURFACE_STYLE_USAGE(.BOTH.,#22250);
#22243=SURFACE_STYLE_USAGE(.BOTH.,#22251);
#22244=SURFACE_STYLE_USAGE(.BOTH.,#22252);
#22245=SURFACE_STYLE_USAGE(.BOTH.,#22253);
#22246=SURFACE_STYLE_USAGE(.BOTH.,#22254);
#22247=SURFACE_SIDE_STYLE('',(#22255));
#22248=SURFACE_SIDE_STYLE('',(#22256));
#22249=SURFACE_SIDE_STYLE('',(#22257));
#22250=SURFACE_SIDE_STYLE('',(#22258));
#22251=SURFACE_SIDE_STYLE('',(#22259));
#22252=SURFACE_SIDE_STYLE('',(#22260));
#22253=SURFACE_SIDE_STYLE('',(#22261));
#22254=SURFACE_SIDE_STYLE('',(#22262));
#22255=SURFACE_STYLE_FILL_AREA(#22263);
#22256=SURFACE_STYLE_FILL_AREA(#22264);
#22257=SURFACE_STYLE_FILL_AREA(#22265);
#22258=SURFACE_STYLE_FILL_AREA(#22266);
#22259=SURFACE_STYLE_FILL_AREA(#22267);
#22260=SURFACE_STYLE_FILL_AREA(#22268);
#22261=SURFACE_STYLE_FILL_AREA(#22269);
#22262=SURFACE_STYLE_FILL_AREA(#22270);
#22263=FILL_AREA_STYLE('Steel - Satin',(#22271));
#22264=FILL_AREA_STYLE('Tool steel gray',(#22272));
#22265=FILL_AREA_STYLE('Pivot dark gray',(#22273));
#22266=FILL_AREA_STYLE('Dark gray',(#22274));
#22267=FILL_AREA_STYLE('Structural dark blue',(#22275));
#22268=FILL_AREA_STYLE('Fastener gray',(#22276));
#22269=FILL_AREA_STYLE('Sky blue soft grip',(#22277));
#22270=FILL_AREA_STYLE('Washer gray',(#22278));
#22271=FILL_AREA_STYLE_COLOUR('Steel - Satin',#22279);
#22272=FILL_AREA_STYLE_COLOUR('Tool steel gray',#22280);
#22273=FILL_AREA_STYLE_COLOUR('Pivot dark gray',#22281);
#22274=FILL_AREA_STYLE_COLOUR('Dark gray',#22282);
#22275=FILL_AREA_STYLE_COLOUR('Structural dark blue',#22283);
#22276=FILL_AREA_STYLE_COLOUR('Fastener gray',#22284);
#22277=FILL_AREA_STYLE_COLOUR('Sky blue soft grip',#22285);
#22278=FILL_AREA_STYLE_COLOUR('Washer gray',#22286);
#22279=COLOUR_RGB('Steel - Satin',0.627450980392157,0.627450980392157,0.627450980392157);
#22280=COLOUR_RGB('Tool steel gray',0.607843137254902,0.643137254901961,
0.698039215686274);
#22281=COLOUR_RGB('Pivot dark gray',0.27843137254902,0.309803921568627,
0.352941176470588);
#22282=COLOUR_RGB('Dark gray',0.250980392156863,0.282352941176471,0.32156862745098);
#22283=COLOUR_RGB('Structural dark blue',0.0901960784313725,0.270588235294118,
0.513725490196078);
#22284=COLOUR_RGB('Fastener gray',0.607843137254902,0.643137254901961,0.698039215686274);
#22285=COLOUR_RGB('Sky blue soft grip',0.317647058823529,0.686274509803922,
0.890196078431372);
#22286=COLOUR_RGB('Washer gray',0.725490196078431,0.752941176470588,0.792156862745098);
ENDSEC;
END-ISO-10303-21;
